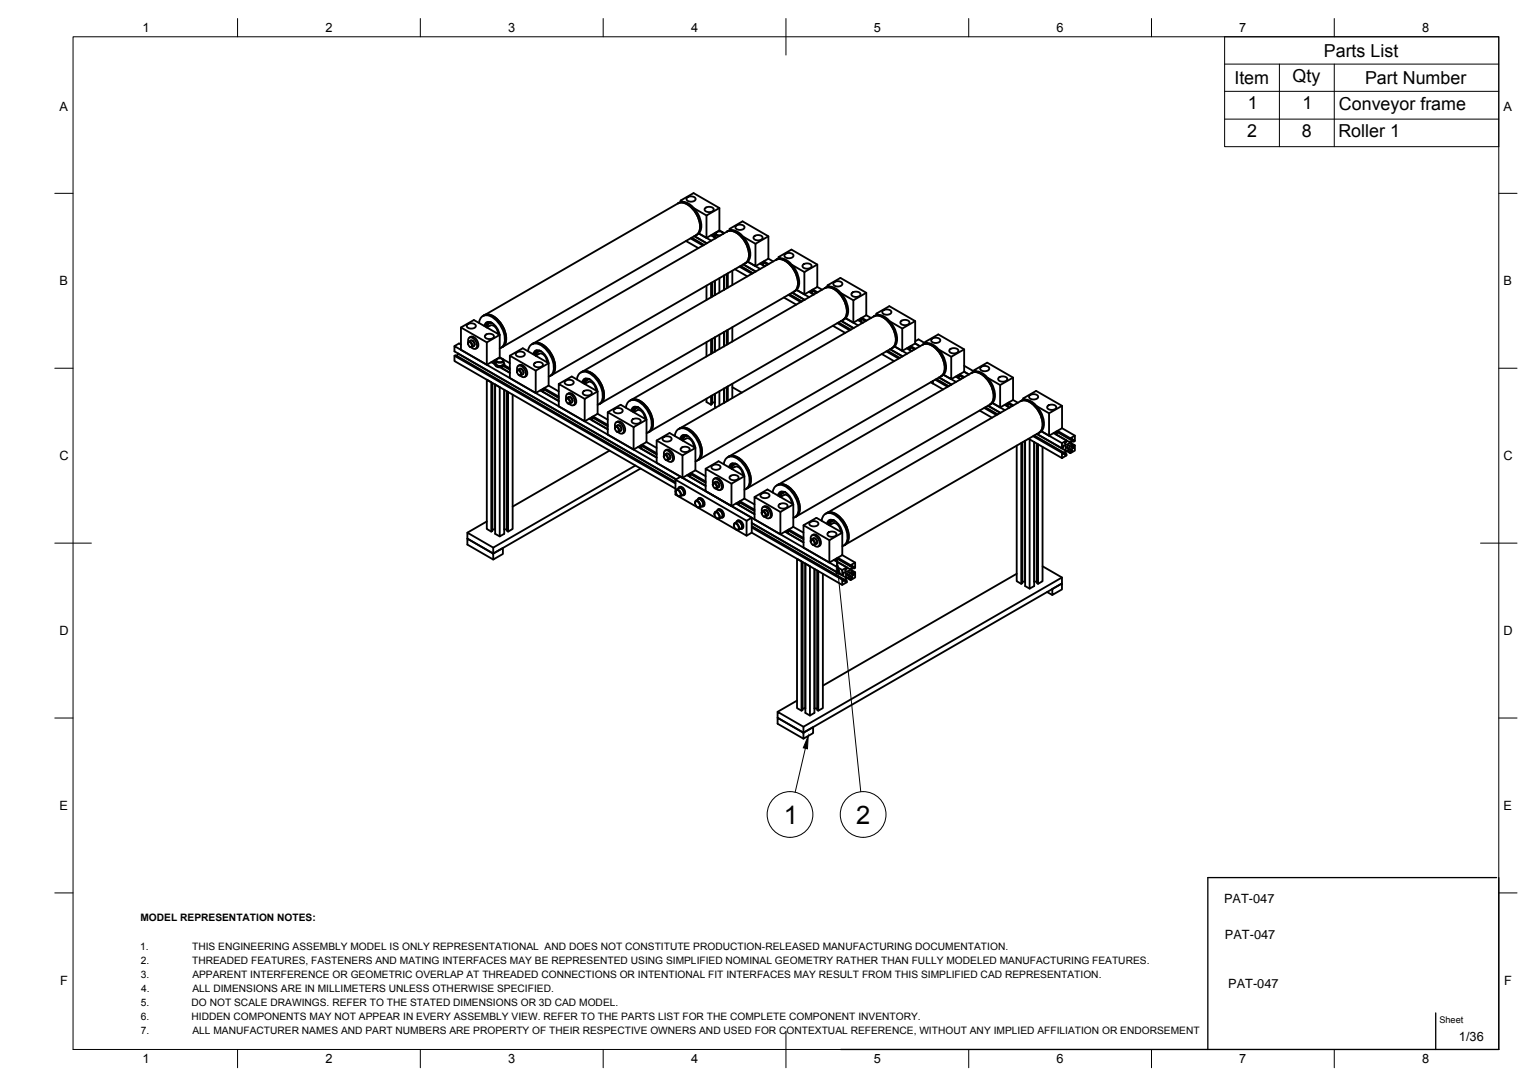
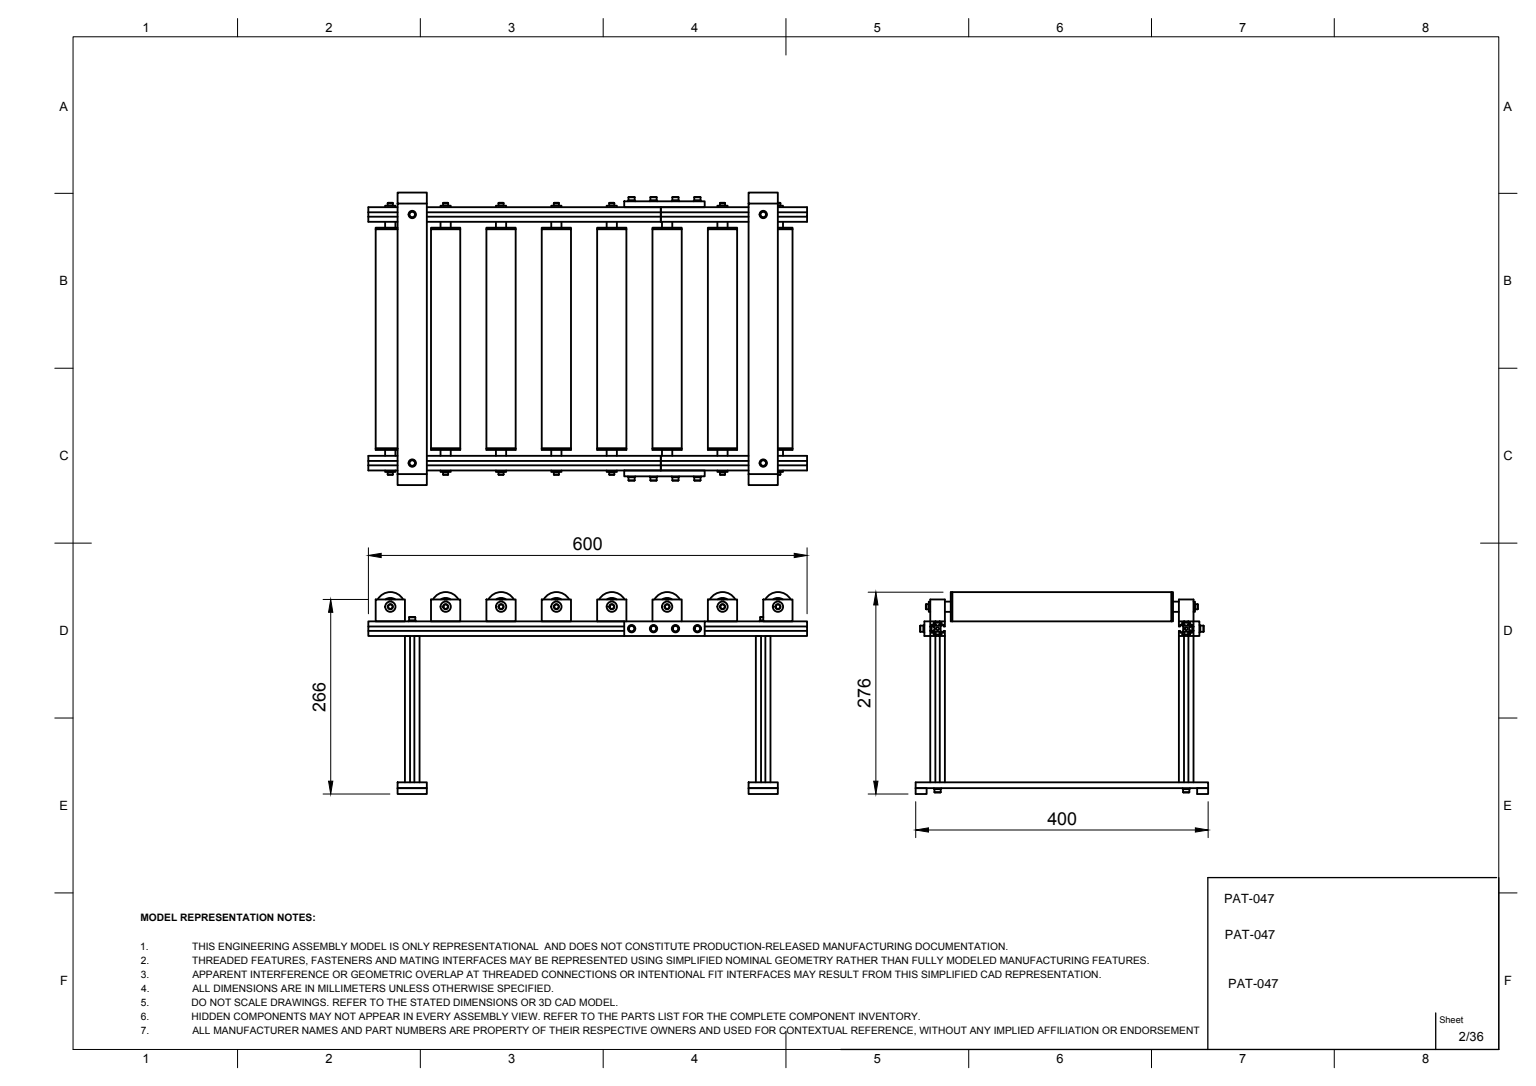
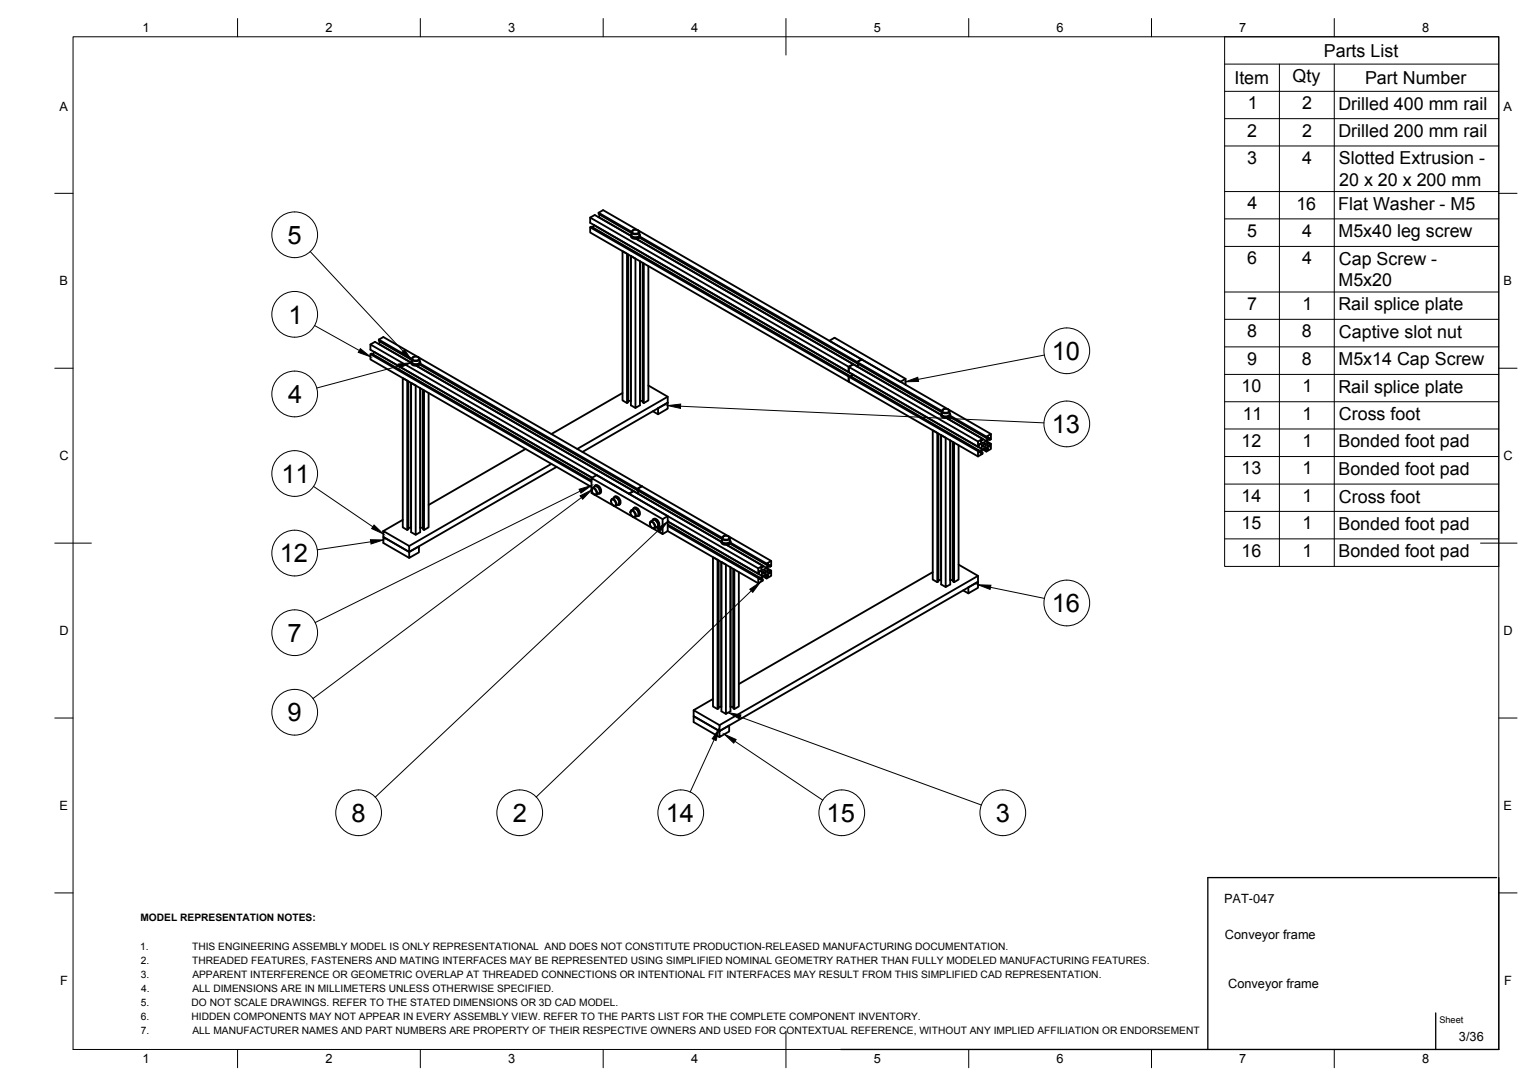
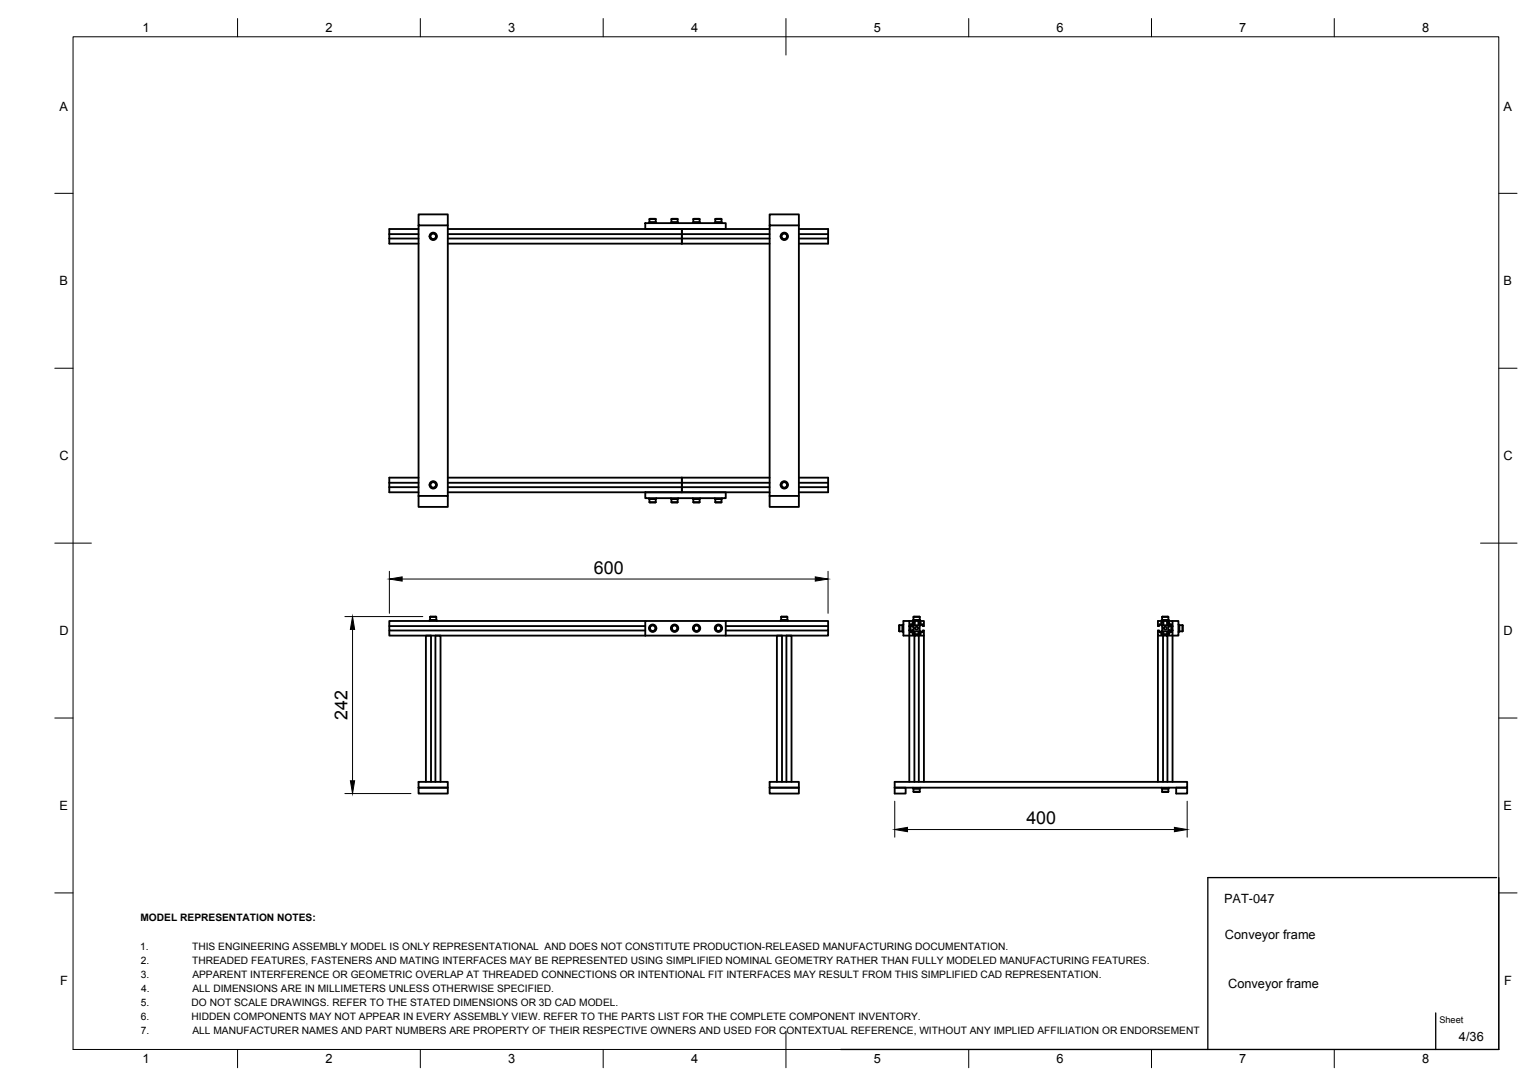
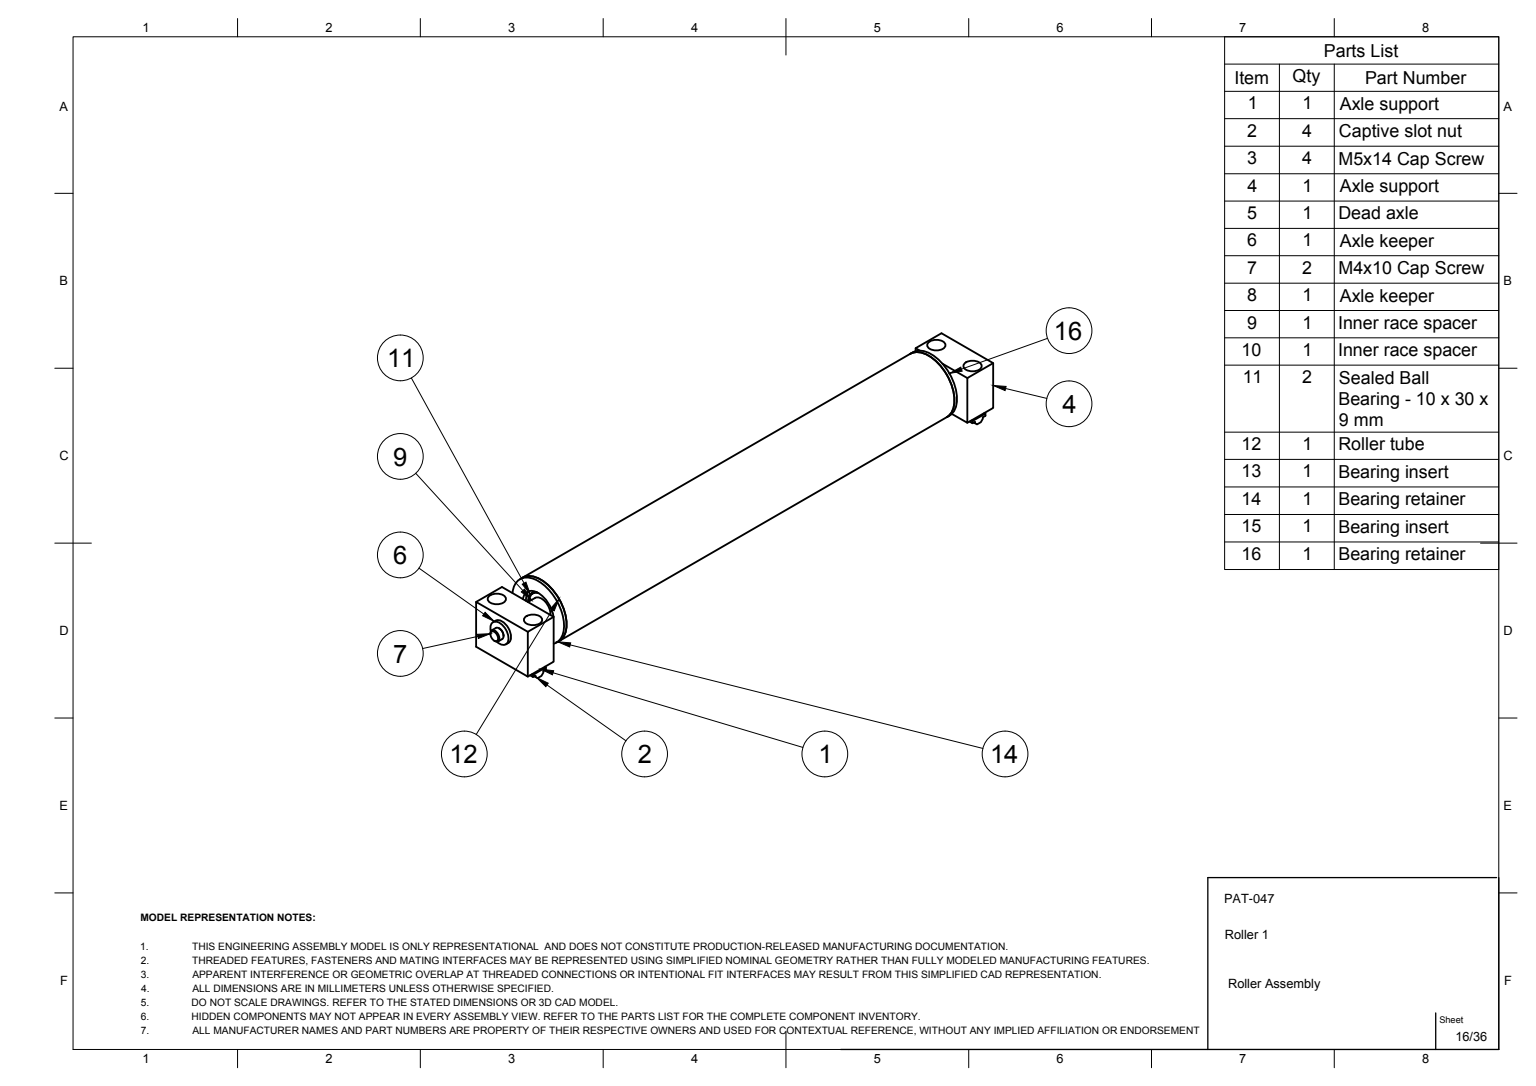
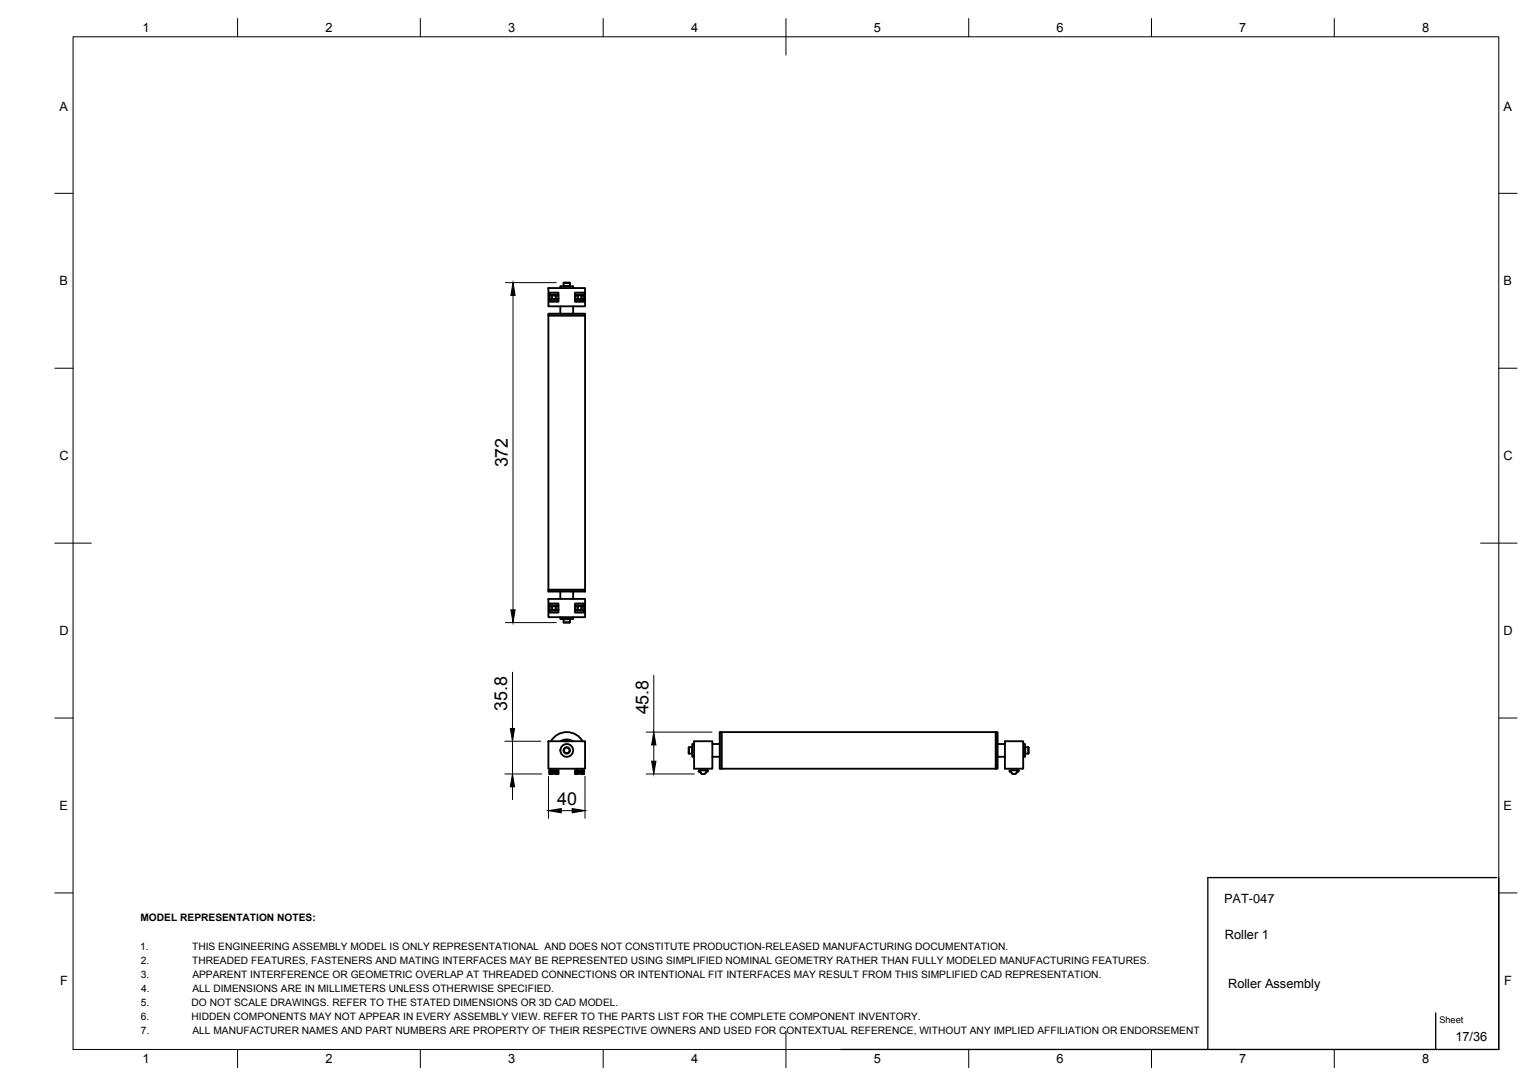
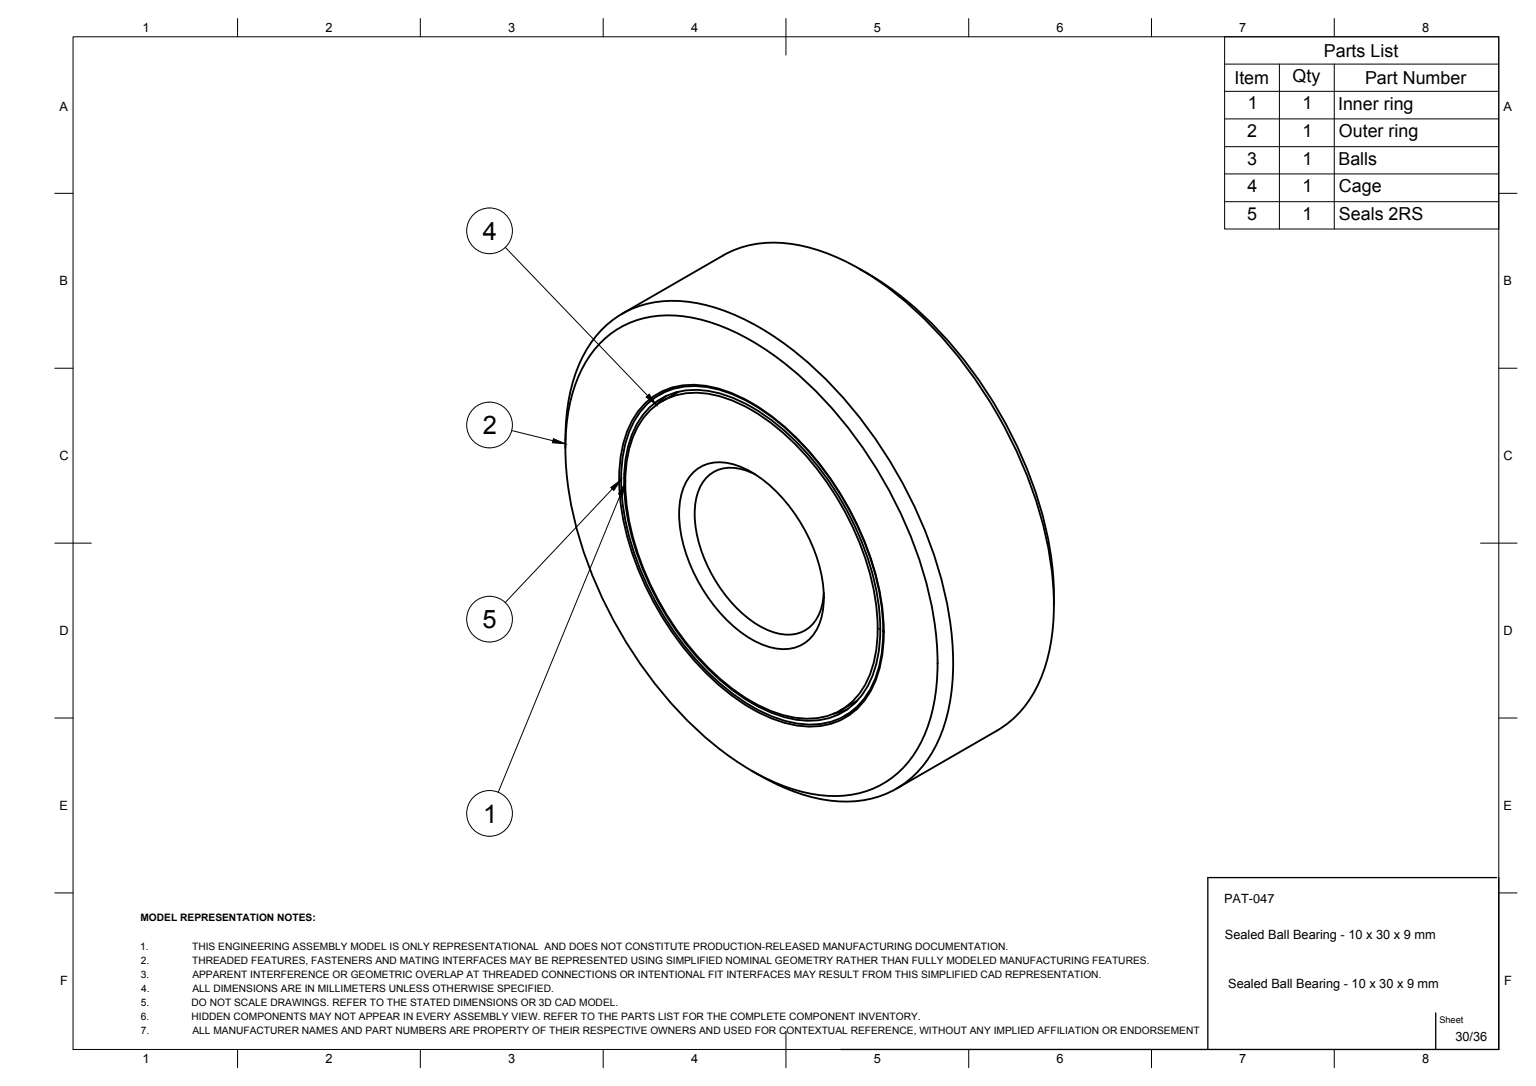
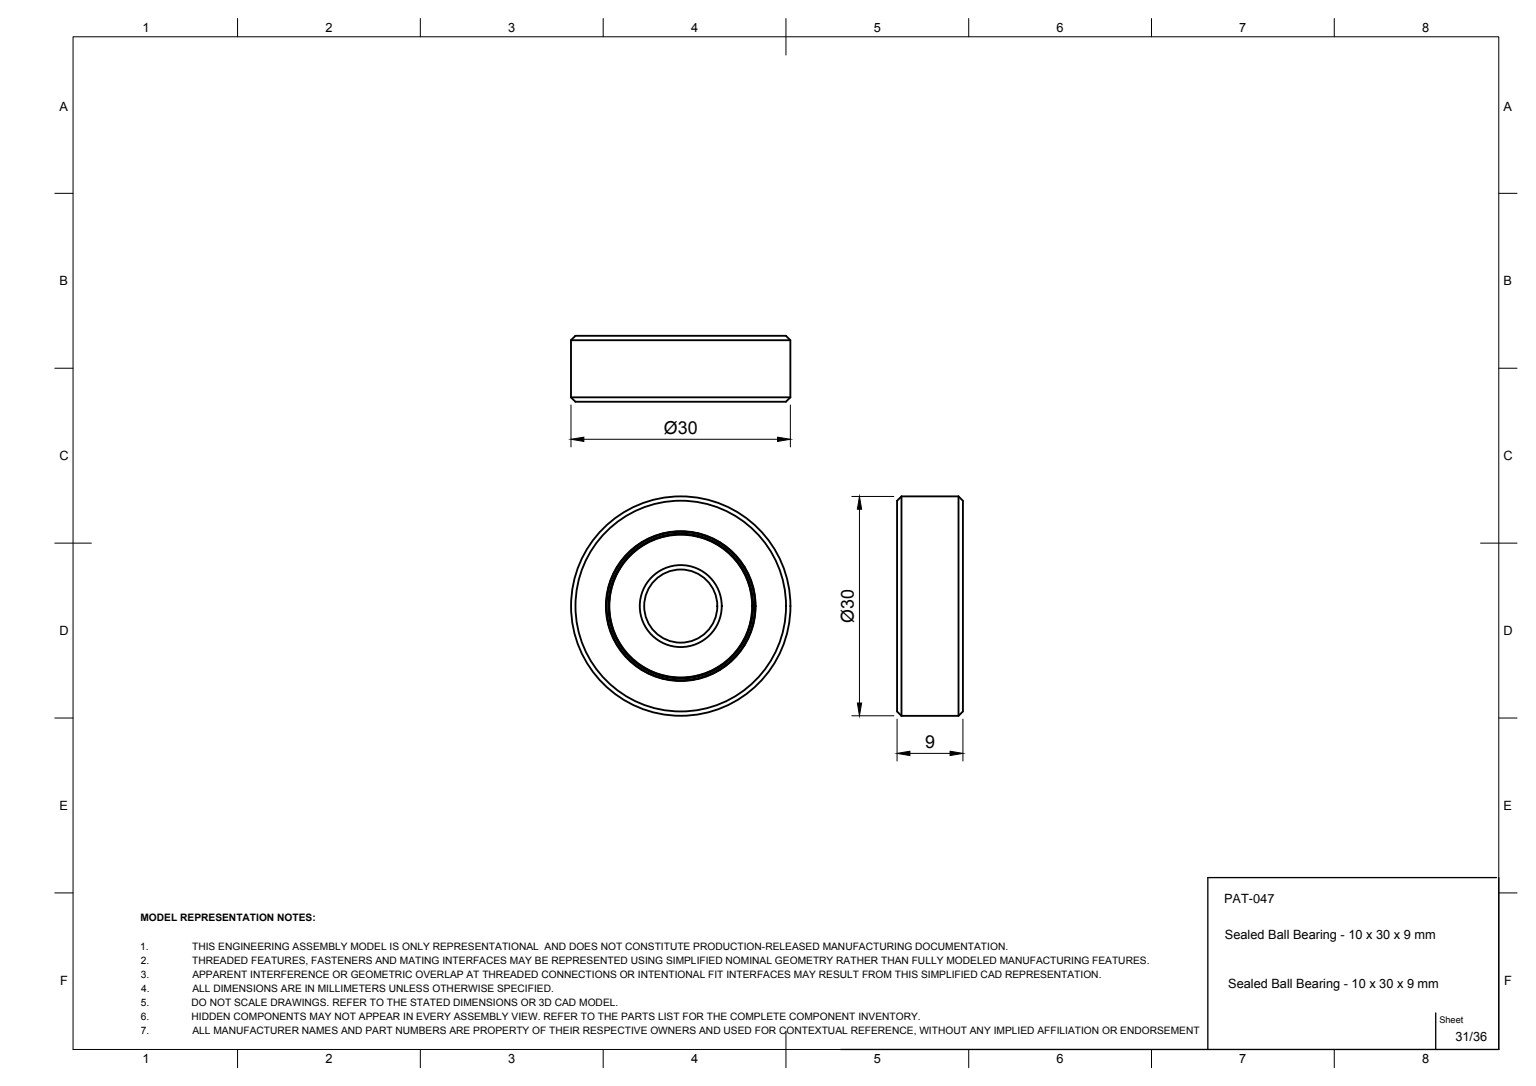
ISO-10303-21;
HEADER;
/* Generated by software containing ST-Developer
 * from STEP Tools, Inc. (www.steptools.com) 
 */

FILE_DESCRIPTION(
/* description */ ('Gravity roller conveyor section'),
/* implementation_level */ '2;1');

FILE_NAME(
/* name */ 'PAT-047',
/* time_stamp */ '2026-11-02T07:43:02-08:00',
/* author */ (''),
/* organization */ (''),
/* preprocessor_version */ 'ST-DEVELOPER v20.2',
/* originating_system */ 'Autodesk Translation Framework v15.17.0.0',
/* authorisation */ '');

FILE_SCHEMA (('AUTOMOTIVE_DESIGN { 1 0 10303 214 3 1 1 }'));
ENDSEC;

DATA;
#10=MECHANICAL_DESIGN_GEOMETRIC_PRESENTATION_REPRESENTATION('',(#529,#530,
#531,#532,#533,#534,#535,#536,#537,#538,#539,#540,#541,#542,#543,#544,#545,
#546,#547,#548,#549,#550,#551,#552,#553,#554,#555,#556,#557,#558,#559,#560,
#561,#562,#563,#564,#565,#566,#567,#568,#569,#570),#13821);
#11=ELLIPSE('',#8670,0.299389011154384,0.2117);
#12=ELLIPSE('',#8674,0.299389011154384,0.2117);
#13=ITEM_DEFINED_TRANSFORMATION($,$,#8484,#8612);
#14=ITEM_DEFINED_TRANSFORMATION($,$,#8504,#8613);
#15=ITEM_DEFINED_TRANSFORMATION($,$,#8524,#8614);
#16=ITEM_DEFINED_TRANSFORMATION($,$,#8541,#8615);
#17=ITEM_DEFINED_TRANSFORMATION($,$,#8595,#8616);
#18=ITEM_DEFINED_TRANSFORMATION($,$,#8069,#8704);
#19=ITEM_DEFINED_TRANSFORMATION($,$,#8123,#8705);
#20=ITEM_DEFINED_TRANSFORMATION($,$,#8177,#8706);
#21=ITEM_DEFINED_TRANSFORMATION($,$,#8300,#8707);
#22=ITEM_DEFINED_TRANSFORMATION($,$,#8227,#8708);
#23=ITEM_DEFINED_TRANSFORMATION($,$,#8300,#8709);
#24=ITEM_DEFINED_TRANSFORMATION($,$,#8255,#8710);
#25=ITEM_DEFINED_TRANSFORMATION($,$,#8177,#8711);
#26=ITEM_DEFINED_TRANSFORMATION($,$,#8300,#8712);
#27=ITEM_DEFINED_TRANSFORMATION($,$,#8227,#8713);
#28=ITEM_DEFINED_TRANSFORMATION($,$,#8300,#8714);
#29=ITEM_DEFINED_TRANSFORMATION($,$,#8255,#8715);
#30=ITEM_DEFINED_TRANSFORMATION($,$,#8050,#8716);
#31=ITEM_DEFINED_TRANSFORMATION($,$,#8659,#8717);
#32=ITEM_DEFINED_TRANSFORMATION($,$,#8300,#8718);
#33=ITEM_DEFINED_TRANSFORMATION($,$,#8680,#8719);
#34=ITEM_DEFINED_TRANSFORMATION($,$,#8659,#8720);
#35=ITEM_DEFINED_TRANSFORMATION($,$,#8300,#8721);
#36=ITEM_DEFINED_TRANSFORMATION($,$,#8680,#8722);
#37=ITEM_DEFINED_TRANSFORMATION($,$,#8659,#8723);
#38=ITEM_DEFINED_TRANSFORMATION($,$,#8300,#8724);
#39=ITEM_DEFINED_TRANSFORMATION($,$,#8680,#8725);
#40=ITEM_DEFINED_TRANSFORMATION($,$,#8659,#8726);
#41=ITEM_DEFINED_TRANSFORMATION($,$,#8300,#8727);
#42=ITEM_DEFINED_TRANSFORMATION($,$,#8680,#8728);
#43=ITEM_DEFINED_TRANSFORMATION($,$,#8069,#8729);
#44=ITEM_DEFINED_TRANSFORMATION($,$,#8123,#8730);
#45=ITEM_DEFINED_TRANSFORMATION($,$,#8177,#8731);
#46=ITEM_DEFINED_TRANSFORMATION($,$,#8300,#8732);
#47=ITEM_DEFINED_TRANSFORMATION($,$,#8227,#8733);
#48=ITEM_DEFINED_TRANSFORMATION($,$,#8300,#8734);
#49=ITEM_DEFINED_TRANSFORMATION($,$,#8255,#8735);
#50=ITEM_DEFINED_TRANSFORMATION($,$,#8177,#8736);
#51=ITEM_DEFINED_TRANSFORMATION($,$,#8300,#8737);
#52=ITEM_DEFINED_TRANSFORMATION($,$,#8227,#8738);
#53=ITEM_DEFINED_TRANSFORMATION($,$,#8300,#8739);
#54=ITEM_DEFINED_TRANSFORMATION($,$,#8255,#8740);
#55=ITEM_DEFINED_TRANSFORMATION($,$,#8281,#8741);
#56=ITEM_DEFINED_TRANSFORMATION($,$,#8659,#8742);
#57=ITEM_DEFINED_TRANSFORMATION($,$,#8300,#8743);
#58=ITEM_DEFINED_TRANSFORMATION($,$,#8680,#8744);
#59=ITEM_DEFINED_TRANSFORMATION($,$,#8659,#8745);
#60=ITEM_DEFINED_TRANSFORMATION($,$,#8300,#8746);
#61=ITEM_DEFINED_TRANSFORMATION($,$,#8680,#8747);
#62=ITEM_DEFINED_TRANSFORMATION($,$,#8659,#8748);
#63=ITEM_DEFINED_TRANSFORMATION($,$,#8300,#8749);
#64=ITEM_DEFINED_TRANSFORMATION($,$,#8680,#8750);
#65=ITEM_DEFINED_TRANSFORMATION($,$,#8659,#8751);
#66=ITEM_DEFINED_TRANSFORMATION($,$,#8300,#8752);
#67=ITEM_DEFINED_TRANSFORMATION($,$,#8680,#8753);
#68=ITEM_DEFINED_TRANSFORMATION($,$,#8311,#8754);
#69=ITEM_DEFINED_TRANSFORMATION($,$,#8324,#8755);
#70=ITEM_DEFINED_TRANSFORMATION($,$,#8331,#8756);
#71=ITEM_DEFINED_TRANSFORMATION($,$,#8338,#8757);
#72=ITEM_DEFINED_TRANSFORMATION($,$,#8351,#8758);
#73=ITEM_DEFINED_TRANSFORMATION($,$,#8358,#8759);
#74=ITEM_DEFINED_TRANSFORMATION($,$,#8366,#8784);
#75=ITEM_DEFINED_TRANSFORMATION($,$,#8375,#8785);
#76=ITEM_DEFINED_TRANSFORMATION($,$,#8388,#8786);
#77=ITEM_DEFINED_TRANSFORMATION($,$,#8401,#8787);
#78=ITEM_DEFINED_TRANSFORMATION($,$,#8414,#8788);
#79=ITEM_DEFINED_TRANSFORMATION($,$,#8427,#8789);
#80=ITEM_DEFINED_TRANSFORMATION($,$,#8441,#8790);
#81=ITEM_DEFINED_TRANSFORMATION($,$,#8465,#8791);
#82=ITEM_DEFINED_TRANSFORMATION($,$,#8474,#8792);
#83=ITEM_DEFINED_TRANSFORMATION($,$,#8483,#8793);
#84=ITEM_DEFINED_TRANSFORMATION($,$,#8626,#8794);
#85=ITEM_DEFINED_TRANSFORMATION($,$,#8659,#8795);
#86=ITEM_DEFINED_TRANSFORMATION($,$,#8680,#8796);
#87=ITEM_DEFINED_TRANSFORMATION($,$,#8680,#8797);
#88=ITEM_DEFINED_TRANSFORMATION($,$,#8659,#8798);
#89=ITEM_DEFINED_TRANSFORMATION($,$,#8483,#8799);
#90=ITEM_DEFINED_TRANSFORMATION($,$,#8617,#8800);
#91=ITEM_DEFINED_TRANSFORMATION($,$,#8626,#8801);
#92=ITEM_DEFINED_TRANSFORMATION($,$,#8650,#8802);
#93=ITEM_DEFINED_TRANSFORMATION($,$,#8659,#8803);
#94=ITEM_DEFINED_TRANSFORMATION($,$,#8680,#8804);
#95=ITEM_DEFINED_TRANSFORMATION($,$,#8659,#8805);
#96=ITEM_DEFINED_TRANSFORMATION($,$,#8680,#8806);
#97=ITEM_DEFINED_TRANSFORMATION($,$,#8760,#8807);
#98=ITEM_DEFINED_TRANSFORMATION($,$,#8049,#8808);
#99=ITEM_DEFINED_TRANSFORMATION($,$,#8365,#8809);
#100=ITEM_DEFINED_TRANSFORMATION($,$,#8365,#8810);
#101=ITEM_DEFINED_TRANSFORMATION($,$,#8365,#8811);
#102=ITEM_DEFINED_TRANSFORMATION($,$,#8365,#8812);
#103=ITEM_DEFINED_TRANSFORMATION($,$,#8365,#8813);
#104=ITEM_DEFINED_TRANSFORMATION($,$,#8365,#8814);
#105=ITEM_DEFINED_TRANSFORMATION($,$,#8365,#8815);
#106=ITEM_DEFINED_TRANSFORMATION($,$,#8365,#8816);
#107=(
REPRESENTATION_RELATIONSHIP($,$,#14023,#14022)
REPRESENTATION_RELATIONSHIP_WITH_TRANSFORMATION(#13)
SHAPE_REPRESENTATION_RELATIONSHIP()
);
#108=(
REPRESENTATION_RELATIONSHIP($,$,#14024,#14022)
REPRESENTATION_RELATIONSHIP_WITH_TRANSFORMATION(#14)
SHAPE_REPRESENTATION_RELATIONSHIP()
);
#109=(
REPRESENTATION_RELATIONSHIP($,$,#14025,#14022)
REPRESENTATION_RELATIONSHIP_WITH_TRANSFORMATION(#15)
SHAPE_REPRESENTATION_RELATIONSHIP()
);
#110=(
REPRESENTATION_RELATIONSHIP($,$,#14026,#14022)
REPRESENTATION_RELATIONSHIP_WITH_TRANSFORMATION(#16)
SHAPE_REPRESENTATION_RELATIONSHIP()
);
#111=(
REPRESENTATION_RELATIONSHIP($,$,#14027,#14022)
REPRESENTATION_RELATIONSHIP_WITH_TRANSFORMATION(#17)
SHAPE_REPRESENTATION_RELATIONSHIP()
);
#112=(
REPRESENTATION_RELATIONSHIP($,$,#13999,#13997)
REPRESENTATION_RELATIONSHIP_WITH_TRANSFORMATION(#18)
SHAPE_REPRESENTATION_RELATIONSHIP()
);
#113=(
REPRESENTATION_RELATIONSHIP($,$,#14000,#13997)
REPRESENTATION_RELATIONSHIP_WITH_TRANSFORMATION(#19)
SHAPE_REPRESENTATION_RELATIONSHIP()
);
#114=(
REPRESENTATION_RELATIONSHIP($,$,#14001,#13997)
REPRESENTATION_RELATIONSHIP_WITH_TRANSFORMATION(#20)
SHAPE_REPRESENTATION_RELATIONSHIP()
);
#115=(
REPRESENTATION_RELATIONSHIP($,$,#14005,#13997)
REPRESENTATION_RELATIONSHIP_WITH_TRANSFORMATION(#21)
SHAPE_REPRESENTATION_RELATIONSHIP()
);
#116=(
REPRESENTATION_RELATIONSHIP($,$,#14002,#13997)
REPRESENTATION_RELATIONSHIP_WITH_TRANSFORMATION(#22)
SHAPE_REPRESENTATION_RELATIONSHIP()
);
#117=(
REPRESENTATION_RELATIONSHIP($,$,#14005,#13997)
REPRESENTATION_RELATIONSHIP_WITH_TRANSFORMATION(#23)
SHAPE_REPRESENTATION_RELATIONSHIP()
);
#118=(
REPRESENTATION_RELATIONSHIP($,$,#14003,#13997)
REPRESENTATION_RELATIONSHIP_WITH_TRANSFORMATION(#24)
SHAPE_REPRESENTATION_RELATIONSHIP()
);
#119=(
REPRESENTATION_RELATIONSHIP($,$,#14001,#13997)
REPRESENTATION_RELATIONSHIP_WITH_TRANSFORMATION(#25)
SHAPE_REPRESENTATION_RELATIONSHIP()
);
#120=(
REPRESENTATION_RELATIONSHIP($,$,#14005,#13997)
REPRESENTATION_RELATIONSHIP_WITH_TRANSFORMATION(#26)
SHAPE_REPRESENTATION_RELATIONSHIP()
);
#121=(
REPRESENTATION_RELATIONSHIP($,$,#14002,#13997)
REPRESENTATION_RELATIONSHIP_WITH_TRANSFORMATION(#27)
SHAPE_REPRESENTATION_RELATIONSHIP()
);
#122=(
REPRESENTATION_RELATIONSHIP($,$,#14005,#13997)
REPRESENTATION_RELATIONSHIP_WITH_TRANSFORMATION(#28)
SHAPE_REPRESENTATION_RELATIONSHIP()
);
#123=(
REPRESENTATION_RELATIONSHIP($,$,#14003,#13997)
REPRESENTATION_RELATIONSHIP_WITH_TRANSFORMATION(#29)
SHAPE_REPRESENTATION_RELATIONSHIP()
);
#124=(
REPRESENTATION_RELATIONSHIP($,$,#13998,#13997)
REPRESENTATION_RELATIONSHIP_WITH_TRANSFORMATION(#30)
SHAPE_REPRESENTATION_RELATIONSHIP()
);
#125=(
REPRESENTATION_RELATIONSHIP($,$,#14031,#13997)
REPRESENTATION_RELATIONSHIP_WITH_TRANSFORMATION(#31)
SHAPE_REPRESENTATION_RELATIONSHIP()
);
#126=(
REPRESENTATION_RELATIONSHIP($,$,#14005,#13997)
REPRESENTATION_RELATIONSHIP_WITH_TRANSFORMATION(#32)
SHAPE_REPRESENTATION_RELATIONSHIP()
);
#127=(
REPRESENTATION_RELATIONSHIP($,$,#14032,#13997)
REPRESENTATION_RELATIONSHIP_WITH_TRANSFORMATION(#33)
SHAPE_REPRESENTATION_RELATIONSHIP()
);
#128=(
REPRESENTATION_RELATIONSHIP($,$,#14031,#13997)
REPRESENTATION_RELATIONSHIP_WITH_TRANSFORMATION(#34)
SHAPE_REPRESENTATION_RELATIONSHIP()
);
#129=(
REPRESENTATION_RELATIONSHIP($,$,#14005,#13997)
REPRESENTATION_RELATIONSHIP_WITH_TRANSFORMATION(#35)
SHAPE_REPRESENTATION_RELATIONSHIP()
);
#130=(
REPRESENTATION_RELATIONSHIP($,$,#14032,#13997)
REPRESENTATION_RELATIONSHIP_WITH_TRANSFORMATION(#36)
SHAPE_REPRESENTATION_RELATIONSHIP()
);
#131=(
REPRESENTATION_RELATIONSHIP($,$,#14031,#13997)
REPRESENTATION_RELATIONSHIP_WITH_TRANSFORMATION(#37)
SHAPE_REPRESENTATION_RELATIONSHIP()
);
#132=(
REPRESENTATION_RELATIONSHIP($,$,#14005,#13997)
REPRESENTATION_RELATIONSHIP_WITH_TRANSFORMATION(#38)
SHAPE_REPRESENTATION_RELATIONSHIP()
);
#133=(
REPRESENTATION_RELATIONSHIP($,$,#14032,#13997)
REPRESENTATION_RELATIONSHIP_WITH_TRANSFORMATION(#39)
SHAPE_REPRESENTATION_RELATIONSHIP()
);
#134=(
REPRESENTATION_RELATIONSHIP($,$,#14031,#13997)
REPRESENTATION_RELATIONSHIP_WITH_TRANSFORMATION(#40)
SHAPE_REPRESENTATION_RELATIONSHIP()
);
#135=(
REPRESENTATION_RELATIONSHIP($,$,#14005,#13997)
REPRESENTATION_RELATIONSHIP_WITH_TRANSFORMATION(#41)
SHAPE_REPRESENTATION_RELATIONSHIP()
);
#136=(
REPRESENTATION_RELATIONSHIP($,$,#14032,#13997)
REPRESENTATION_RELATIONSHIP_WITH_TRANSFORMATION(#42)
SHAPE_REPRESENTATION_RELATIONSHIP()
);
#137=(
REPRESENTATION_RELATIONSHIP($,$,#13999,#13997)
REPRESENTATION_RELATIONSHIP_WITH_TRANSFORMATION(#43)
SHAPE_REPRESENTATION_RELATIONSHIP()
);
#138=(
REPRESENTATION_RELATIONSHIP($,$,#14000,#13997)
REPRESENTATION_RELATIONSHIP_WITH_TRANSFORMATION(#44)
SHAPE_REPRESENTATION_RELATIONSHIP()
);
#139=(
REPRESENTATION_RELATIONSHIP($,$,#14001,#13997)
REPRESENTATION_RELATIONSHIP_WITH_TRANSFORMATION(#45)
SHAPE_REPRESENTATION_RELATIONSHIP()
);
#140=(
REPRESENTATION_RELATIONSHIP($,$,#14005,#13997)
REPRESENTATION_RELATIONSHIP_WITH_TRANSFORMATION(#46)
SHAPE_REPRESENTATION_RELATIONSHIP()
);
#141=(
REPRESENTATION_RELATIONSHIP($,$,#14002,#13997)
REPRESENTATION_RELATIONSHIP_WITH_TRANSFORMATION(#47)
SHAPE_REPRESENTATION_RELATIONSHIP()
);
#142=(
REPRESENTATION_RELATIONSHIP($,$,#14005,#13997)
REPRESENTATION_RELATIONSHIP_WITH_TRANSFORMATION(#48)
SHAPE_REPRESENTATION_RELATIONSHIP()
);
#143=(
REPRESENTATION_RELATIONSHIP($,$,#14003,#13997)
REPRESENTATION_RELATIONSHIP_WITH_TRANSFORMATION(#49)
SHAPE_REPRESENTATION_RELATIONSHIP()
);
#144=(
REPRESENTATION_RELATIONSHIP($,$,#14001,#13997)
REPRESENTATION_RELATIONSHIP_WITH_TRANSFORMATION(#50)
SHAPE_REPRESENTATION_RELATIONSHIP()
);
#145=(
REPRESENTATION_RELATIONSHIP($,$,#14005,#13997)
REPRESENTATION_RELATIONSHIP_WITH_TRANSFORMATION(#51)
SHAPE_REPRESENTATION_RELATIONSHIP()
);
#146=(
REPRESENTATION_RELATIONSHIP($,$,#14002,#13997)
REPRESENTATION_RELATIONSHIP_WITH_TRANSFORMATION(#52)
SHAPE_REPRESENTATION_RELATIONSHIP()
);
#147=(
REPRESENTATION_RELATIONSHIP($,$,#14005,#13997)
REPRESENTATION_RELATIONSHIP_WITH_TRANSFORMATION(#53)
SHAPE_REPRESENTATION_RELATIONSHIP()
);
#148=(
REPRESENTATION_RELATIONSHIP($,$,#14003,#13997)
REPRESENTATION_RELATIONSHIP_WITH_TRANSFORMATION(#54)
SHAPE_REPRESENTATION_RELATIONSHIP()
);
#149=(
REPRESENTATION_RELATIONSHIP($,$,#14004,#13997)
REPRESENTATION_RELATIONSHIP_WITH_TRANSFORMATION(#55)
SHAPE_REPRESENTATION_RELATIONSHIP()
);
#150=(
REPRESENTATION_RELATIONSHIP($,$,#14031,#13997)
REPRESENTATION_RELATIONSHIP_WITH_TRANSFORMATION(#56)
SHAPE_REPRESENTATION_RELATIONSHIP()
);
#151=(
REPRESENTATION_RELATIONSHIP($,$,#14005,#13997)
REPRESENTATION_RELATIONSHIP_WITH_TRANSFORMATION(#57)
SHAPE_REPRESENTATION_RELATIONSHIP()
);
#152=(
REPRESENTATION_RELATIONSHIP($,$,#14032,#13997)
REPRESENTATION_RELATIONSHIP_WITH_TRANSFORMATION(#58)
SHAPE_REPRESENTATION_RELATIONSHIP()
);
#153=(
REPRESENTATION_RELATIONSHIP($,$,#14031,#13997)
REPRESENTATION_RELATIONSHIP_WITH_TRANSFORMATION(#59)
SHAPE_REPRESENTATION_RELATIONSHIP()
);
#154=(
REPRESENTATION_RELATIONSHIP($,$,#14005,#13997)
REPRESENTATION_RELATIONSHIP_WITH_TRANSFORMATION(#60)
SHAPE_REPRESENTATION_RELATIONSHIP()
);
#155=(
REPRESENTATION_RELATIONSHIP($,$,#14032,#13997)
REPRESENTATION_RELATIONSHIP_WITH_TRANSFORMATION(#61)
SHAPE_REPRESENTATION_RELATIONSHIP()
);
#156=(
REPRESENTATION_RELATIONSHIP($,$,#14031,#13997)
REPRESENTATION_RELATIONSHIP_WITH_TRANSFORMATION(#62)
SHAPE_REPRESENTATION_RELATIONSHIP()
);
#157=(
REPRESENTATION_RELATIONSHIP($,$,#14005,#13997)
REPRESENTATION_RELATIONSHIP_WITH_TRANSFORMATION(#63)
SHAPE_REPRESENTATION_RELATIONSHIP()
);
#158=(
REPRESENTATION_RELATIONSHIP($,$,#14032,#13997)
REPRESENTATION_RELATIONSHIP_WITH_TRANSFORMATION(#64)
SHAPE_REPRESENTATION_RELATIONSHIP()
);
#159=(
REPRESENTATION_RELATIONSHIP($,$,#14031,#13997)
REPRESENTATION_RELATIONSHIP_WITH_TRANSFORMATION(#65)
SHAPE_REPRESENTATION_RELATIONSHIP()
);
#160=(
REPRESENTATION_RELATIONSHIP($,$,#14005,#13997)
REPRESENTATION_RELATIONSHIP_WITH_TRANSFORMATION(#66)
SHAPE_REPRESENTATION_RELATIONSHIP()
);
#161=(
REPRESENTATION_RELATIONSHIP($,$,#14032,#13997)
REPRESENTATION_RELATIONSHIP_WITH_TRANSFORMATION(#67)
SHAPE_REPRESENTATION_RELATIONSHIP()
);
#162=(
REPRESENTATION_RELATIONSHIP($,$,#14006,#13997)
REPRESENTATION_RELATIONSHIP_WITH_TRANSFORMATION(#68)
SHAPE_REPRESENTATION_RELATIONSHIP()
);
#163=(
REPRESENTATION_RELATIONSHIP($,$,#14007,#13997)
REPRESENTATION_RELATIONSHIP_WITH_TRANSFORMATION(#69)
SHAPE_REPRESENTATION_RELATIONSHIP()
);
#164=(
REPRESENTATION_RELATIONSHIP($,$,#14008,#13997)
REPRESENTATION_RELATIONSHIP_WITH_TRANSFORMATION(#70)
SHAPE_REPRESENTATION_RELATIONSHIP()
);
#165=(
REPRESENTATION_RELATIONSHIP($,$,#14009,#13997)
REPRESENTATION_RELATIONSHIP_WITH_TRANSFORMATION(#71)
SHAPE_REPRESENTATION_RELATIONSHIP()
);
#166=(
REPRESENTATION_RELATIONSHIP($,$,#14010,#13997)
REPRESENTATION_RELATIONSHIP_WITH_TRANSFORMATION(#72)
SHAPE_REPRESENTATION_RELATIONSHIP()
);
#167=(
REPRESENTATION_RELATIONSHIP($,$,#14011,#13997)
REPRESENTATION_RELATIONSHIP_WITH_TRANSFORMATION(#73)
SHAPE_REPRESENTATION_RELATIONSHIP()
);
#168=(
REPRESENTATION_RELATIONSHIP($,$,#14013,#14012)
REPRESENTATION_RELATIONSHIP_WITH_TRANSFORMATION(#74)
SHAPE_REPRESENTATION_RELATIONSHIP()
);
#169=(
REPRESENTATION_RELATIONSHIP($,$,#14014,#14012)
REPRESENTATION_RELATIONSHIP_WITH_TRANSFORMATION(#75)
SHAPE_REPRESENTATION_RELATIONSHIP()
);
#170=(
REPRESENTATION_RELATIONSHIP($,$,#14015,#14012)
REPRESENTATION_RELATIONSHIP_WITH_TRANSFORMATION(#76)
SHAPE_REPRESENTATION_RELATIONSHIP()
);
#171=(
REPRESENTATION_RELATIONSHIP($,$,#14016,#14012)
REPRESENTATION_RELATIONSHIP_WITH_TRANSFORMATION(#77)
SHAPE_REPRESENTATION_RELATIONSHIP()
);
#172=(
REPRESENTATION_RELATIONSHIP($,$,#14017,#14012)
REPRESENTATION_RELATIONSHIP_WITH_TRANSFORMATION(#78)
SHAPE_REPRESENTATION_RELATIONSHIP()
);
#173=(
REPRESENTATION_RELATIONSHIP($,$,#14018,#14012)
REPRESENTATION_RELATIONSHIP_WITH_TRANSFORMATION(#79)
SHAPE_REPRESENTATION_RELATIONSHIP()
);
#174=(
REPRESENTATION_RELATIONSHIP($,$,#14019,#14012)
REPRESENTATION_RELATIONSHIP_WITH_TRANSFORMATION(#80)
SHAPE_REPRESENTATION_RELATIONSHIP()
);
#175=(
REPRESENTATION_RELATIONSHIP($,$,#14020,#14012)
REPRESENTATION_RELATIONSHIP_WITH_TRANSFORMATION(#81)
SHAPE_REPRESENTATION_RELATIONSHIP()
);
#176=(
REPRESENTATION_RELATIONSHIP($,$,#14021,#14012)
REPRESENTATION_RELATIONSHIP_WITH_TRANSFORMATION(#82)
SHAPE_REPRESENTATION_RELATIONSHIP()
);
#177=(
REPRESENTATION_RELATIONSHIP($,$,#14022,#14012)
REPRESENTATION_RELATIONSHIP_WITH_TRANSFORMATION(#83)
SHAPE_REPRESENTATION_RELATIONSHIP()
);
#178=(
REPRESENTATION_RELATIONSHIP($,$,#14029,#14012)
REPRESENTATION_RELATIONSHIP_WITH_TRANSFORMATION(#84)
SHAPE_REPRESENTATION_RELATIONSHIP()
);
#179=(
REPRESENTATION_RELATIONSHIP($,$,#14031,#14012)
REPRESENTATION_RELATIONSHIP_WITH_TRANSFORMATION(#85)
SHAPE_REPRESENTATION_RELATIONSHIP()
);
#180=(
REPRESENTATION_RELATIONSHIP($,$,#14032,#14012)
REPRESENTATION_RELATIONSHIP_WITH_TRANSFORMATION(#86)
SHAPE_REPRESENTATION_RELATIONSHIP()
);
#181=(
REPRESENTATION_RELATIONSHIP($,$,#14032,#14012)
REPRESENTATION_RELATIONSHIP_WITH_TRANSFORMATION(#87)
SHAPE_REPRESENTATION_RELATIONSHIP()
);
#182=(
REPRESENTATION_RELATIONSHIP($,$,#14031,#14012)
REPRESENTATION_RELATIONSHIP_WITH_TRANSFORMATION(#88)
SHAPE_REPRESENTATION_RELATIONSHIP()
);
#183=(
REPRESENTATION_RELATIONSHIP($,$,#14022,#14012)
REPRESENTATION_RELATIONSHIP_WITH_TRANSFORMATION(#89)
SHAPE_REPRESENTATION_RELATIONSHIP()
);
#184=(
REPRESENTATION_RELATIONSHIP($,$,#14028,#14012)
REPRESENTATION_RELATIONSHIP_WITH_TRANSFORMATION(#90)
SHAPE_REPRESENTATION_RELATIONSHIP()
);
#185=(
REPRESENTATION_RELATIONSHIP($,$,#14029,#14012)
REPRESENTATION_RELATIONSHIP_WITH_TRANSFORMATION(#91)
SHAPE_REPRESENTATION_RELATIONSHIP()
);
#186=(
REPRESENTATION_RELATIONSHIP($,$,#14030,#14012)
REPRESENTATION_RELATIONSHIP_WITH_TRANSFORMATION(#92)
SHAPE_REPRESENTATION_RELATIONSHIP()
);
#187=(
REPRESENTATION_RELATIONSHIP($,$,#14031,#14012)
REPRESENTATION_RELATIONSHIP_WITH_TRANSFORMATION(#93)
SHAPE_REPRESENTATION_RELATIONSHIP()
);
#188=(
REPRESENTATION_RELATIONSHIP($,$,#14032,#14012)
REPRESENTATION_RELATIONSHIP_WITH_TRANSFORMATION(#94)
SHAPE_REPRESENTATION_RELATIONSHIP()
);
#189=(
REPRESENTATION_RELATIONSHIP($,$,#14031,#14012)
REPRESENTATION_RELATIONSHIP_WITH_TRANSFORMATION(#95)
SHAPE_REPRESENTATION_RELATIONSHIP()
);
#190=(
REPRESENTATION_RELATIONSHIP($,$,#14032,#14012)
REPRESENTATION_RELATIONSHIP_WITH_TRANSFORMATION(#96)
SHAPE_REPRESENTATION_RELATIONSHIP()
);
#191=(
REPRESENTATION_RELATIONSHIP($,$,#14033,#14012)
REPRESENTATION_RELATIONSHIP_WITH_TRANSFORMATION(#97)
SHAPE_REPRESENTATION_RELATIONSHIP()
);
#192=(
REPRESENTATION_RELATIONSHIP($,$,#13997,#13996)
REPRESENTATION_RELATIONSHIP_WITH_TRANSFORMATION(#98)
SHAPE_REPRESENTATION_RELATIONSHIP()
);
#193=(
REPRESENTATION_RELATIONSHIP($,$,#14012,#13996)
REPRESENTATION_RELATIONSHIP_WITH_TRANSFORMATION(#99)
SHAPE_REPRESENTATION_RELATIONSHIP()
);
#194=(
REPRESENTATION_RELATIONSHIP($,$,#14012,#13996)
REPRESENTATION_RELATIONSHIP_WITH_TRANSFORMATION(#100)
SHAPE_REPRESENTATION_RELATIONSHIP()
);
#195=(
REPRESENTATION_RELATIONSHIP($,$,#14012,#13996)
REPRESENTATION_RELATIONSHIP_WITH_TRANSFORMATION(#101)
SHAPE_REPRESENTATION_RELATIONSHIP()
);
#196=(
REPRESENTATION_RELATIONSHIP($,$,#14012,#13996)
REPRESENTATION_RELATIONSHIP_WITH_TRANSFORMATION(#102)
SHAPE_REPRESENTATION_RELATIONSHIP()
);
#197=(
REPRESENTATION_RELATIONSHIP($,$,#14012,#13996)
REPRESENTATION_RELATIONSHIP_WITH_TRANSFORMATION(#103)
SHAPE_REPRESENTATION_RELATIONSHIP()
);
#198=(
REPRESENTATION_RELATIONSHIP($,$,#14012,#13996)
REPRESENTATION_RELATIONSHIP_WITH_TRANSFORMATION(#104)
SHAPE_REPRESENTATION_RELATIONSHIP()
);
#199=(
REPRESENTATION_RELATIONSHIP($,$,#14012,#13996)
REPRESENTATION_RELATIONSHIP_WITH_TRANSFORMATION(#105)
SHAPE_REPRESENTATION_RELATIONSHIP()
);
#200=(
REPRESENTATION_RELATIONSHIP($,$,#14012,#13996)
REPRESENTATION_RELATIONSHIP_WITH_TRANSFORMATION(#106)
SHAPE_REPRESENTATION_RELATIONSHIP()
);
#201=CONTEXT_DEPENDENT_SHAPE_REPRESENTATION(#107,#13896);
#202=CONTEXT_DEPENDENT_SHAPE_REPRESENTATION(#108,#13897);
#203=CONTEXT_DEPENDENT_SHAPE_REPRESENTATION(#109,#13898);
#204=CONTEXT_DEPENDENT_SHAPE_REPRESENTATION(#110,#13899);
#205=CONTEXT_DEPENDENT_SHAPE_REPRESENTATION(#111,#13900);
#206=CONTEXT_DEPENDENT_SHAPE_REPRESENTATION(#112,#13906);
#207=CONTEXT_DEPENDENT_SHAPE_REPRESENTATION(#113,#13907);
#208=CONTEXT_DEPENDENT_SHAPE_REPRESENTATION(#114,#13908);
#209=CONTEXT_DEPENDENT_SHAPE_REPRESENTATION(#115,#13909);
#210=CONTEXT_DEPENDENT_SHAPE_REPRESENTATION(#116,#13910);
#211=CONTEXT_DEPENDENT_SHAPE_REPRESENTATION(#117,#13911);
#212=CONTEXT_DEPENDENT_SHAPE_REPRESENTATION(#118,#13912);
#213=CONTEXT_DEPENDENT_SHAPE_REPRESENTATION(#119,#13913);
#214=CONTEXT_DEPENDENT_SHAPE_REPRESENTATION(#120,#13914);
#215=CONTEXT_DEPENDENT_SHAPE_REPRESENTATION(#121,#13915);
#216=CONTEXT_DEPENDENT_SHAPE_REPRESENTATION(#122,#13916);
#217=CONTEXT_DEPENDENT_SHAPE_REPRESENTATION(#123,#13917);
#218=CONTEXT_DEPENDENT_SHAPE_REPRESENTATION(#124,#13918);
#219=CONTEXT_DEPENDENT_SHAPE_REPRESENTATION(#125,#13919);
#220=CONTEXT_DEPENDENT_SHAPE_REPRESENTATION(#126,#13920);
#221=CONTEXT_DEPENDENT_SHAPE_REPRESENTATION(#127,#13921);
#222=CONTEXT_DEPENDENT_SHAPE_REPRESENTATION(#128,#13922);
#223=CONTEXT_DEPENDENT_SHAPE_REPRESENTATION(#129,#13923);
#224=CONTEXT_DEPENDENT_SHAPE_REPRESENTATION(#130,#13924);
#225=CONTEXT_DEPENDENT_SHAPE_REPRESENTATION(#131,#13925);
#226=CONTEXT_DEPENDENT_SHAPE_REPRESENTATION(#132,#13926);
#227=CONTEXT_DEPENDENT_SHAPE_REPRESENTATION(#133,#13927);
#228=CONTEXT_DEPENDENT_SHAPE_REPRESENTATION(#134,#13928);
#229=CONTEXT_DEPENDENT_SHAPE_REPRESENTATION(#135,#13929);
#230=CONTEXT_DEPENDENT_SHAPE_REPRESENTATION(#136,#13930);
#231=CONTEXT_DEPENDENT_SHAPE_REPRESENTATION(#137,#13931);
#232=CONTEXT_DEPENDENT_SHAPE_REPRESENTATION(#138,#13932);
#233=CONTEXT_DEPENDENT_SHAPE_REPRESENTATION(#139,#13933);
#234=CONTEXT_DEPENDENT_SHAPE_REPRESENTATION(#140,#13934);
#235=CONTEXT_DEPENDENT_SHAPE_REPRESENTATION(#141,#13935);
#236=CONTEXT_DEPENDENT_SHAPE_REPRESENTATION(#142,#13936);
#237=CONTEXT_DEPENDENT_SHAPE_REPRESENTATION(#143,#13937);
#238=CONTEXT_DEPENDENT_SHAPE_REPRESENTATION(#144,#13938);
#239=CONTEXT_DEPENDENT_SHAPE_REPRESENTATION(#145,#13939);
#240=CONTEXT_DEPENDENT_SHAPE_REPRESENTATION(#146,#13940);
#241=CONTEXT_DEPENDENT_SHAPE_REPRESENTATION(#147,#13941);
#242=CONTEXT_DEPENDENT_SHAPE_REPRESENTATION(#148,#13942);
#243=CONTEXT_DEPENDENT_SHAPE_REPRESENTATION(#149,#13943);
#244=CONTEXT_DEPENDENT_SHAPE_REPRESENTATION(#150,#13944);
#245=CONTEXT_DEPENDENT_SHAPE_REPRESENTATION(#151,#13945);
#246=CONTEXT_DEPENDENT_SHAPE_REPRESENTATION(#152,#13946);
#247=CONTEXT_DEPENDENT_SHAPE_REPRESENTATION(#153,#13947);
#248=CONTEXT_DEPENDENT_SHAPE_REPRESENTATION(#154,#13948);
#249=CONTEXT_DEPENDENT_SHAPE_REPRESENTATION(#155,#13949);
#250=CONTEXT_DEPENDENT_SHAPE_REPRESENTATION(#156,#13950);
#251=CONTEXT_DEPENDENT_SHAPE_REPRESENTATION(#157,#13951);
#252=CONTEXT_DEPENDENT_SHAPE_REPRESENTATION(#158,#13952);
#253=CONTEXT_DEPENDENT_SHAPE_REPRESENTATION(#159,#13953);
#254=CONTEXT_DEPENDENT_SHAPE_REPRESENTATION(#160,#13954);
#255=CONTEXT_DEPENDENT_SHAPE_REPRESENTATION(#161,#13955);
#256=CONTEXT_DEPENDENT_SHAPE_REPRESENTATION(#162,#13956);
#257=CONTEXT_DEPENDENT_SHAPE_REPRESENTATION(#163,#13957);
#258=CONTEXT_DEPENDENT_SHAPE_REPRESENTATION(#164,#13958);
#259=CONTEXT_DEPENDENT_SHAPE_REPRESENTATION(#165,#13959);
#260=CONTEXT_DEPENDENT_SHAPE_REPRESENTATION(#166,#13960);
#261=CONTEXT_DEPENDENT_SHAPE_REPRESENTATION(#167,#13961);
#262=CONTEXT_DEPENDENT_SHAPE_REPRESENTATION(#168,#13963);
#263=CONTEXT_DEPENDENT_SHAPE_REPRESENTATION(#169,#13964);
#264=CONTEXT_DEPENDENT_SHAPE_REPRESENTATION(#170,#13965);
#265=CONTEXT_DEPENDENT_SHAPE_REPRESENTATION(#171,#13966);
#266=CONTEXT_DEPENDENT_SHAPE_REPRESENTATION(#172,#13967);
#267=CONTEXT_DEPENDENT_SHAPE_REPRESENTATION(#173,#13968);
#268=CONTEXT_DEPENDENT_SHAPE_REPRESENTATION(#174,#13969);
#269=CONTEXT_DEPENDENT_SHAPE_REPRESENTATION(#175,#13970);
#270=CONTEXT_DEPENDENT_SHAPE_REPRESENTATION(#176,#13971);
#271=CONTEXT_DEPENDENT_SHAPE_REPRESENTATION(#177,#13972);
#272=CONTEXT_DEPENDENT_SHAPE_REPRESENTATION(#178,#13973);
#273=CONTEXT_DEPENDENT_SHAPE_REPRESENTATION(#179,#13974);
#274=CONTEXT_DEPENDENT_SHAPE_REPRESENTATION(#180,#13975);
#275=CONTEXT_DEPENDENT_SHAPE_REPRESENTATION(#181,#13976);
#276=CONTEXT_DEPENDENT_SHAPE_REPRESENTATION(#182,#13977);
#277=CONTEXT_DEPENDENT_SHAPE_REPRESENTATION(#183,#13978);
#278=CONTEXT_DEPENDENT_SHAPE_REPRESENTATION(#184,#13979);
#279=CONTEXT_DEPENDENT_SHAPE_REPRESENTATION(#185,#13980);
#280=CONTEXT_DEPENDENT_SHAPE_REPRESENTATION(#186,#13981);
#281=CONTEXT_DEPENDENT_SHAPE_REPRESENTATION(#187,#13982);
#282=CONTEXT_DEPENDENT_SHAPE_REPRESENTATION(#188,#13983);
#283=CONTEXT_DEPENDENT_SHAPE_REPRESENTATION(#189,#13984);
#284=CONTEXT_DEPENDENT_SHAPE_REPRESENTATION(#190,#13985);
#285=CONTEXT_DEPENDENT_SHAPE_REPRESENTATION(#191,#13986);
#286=CONTEXT_DEPENDENT_SHAPE_REPRESENTATION(#192,#13987);
#287=CONTEXT_DEPENDENT_SHAPE_REPRESENTATION(#193,#13988);
#288=CONTEXT_DEPENDENT_SHAPE_REPRESENTATION(#194,#13989);
#289=CONTEXT_DEPENDENT_SHAPE_REPRESENTATION(#195,#13990);
#290=CONTEXT_DEPENDENT_SHAPE_REPRESENTATION(#196,#13991);
#291=CONTEXT_DEPENDENT_SHAPE_REPRESENTATION(#197,#13992);
#292=CONTEXT_DEPENDENT_SHAPE_REPRESENTATION(#198,#13993);
#293=CONTEXT_DEPENDENT_SHAPE_REPRESENTATION(#199,#13994);
#294=CONTEXT_DEPENDENT_SHAPE_REPRESENTATION(#200,#13995);
#295=NEXT_ASSEMBLY_USAGE_OCCURRENCE('Inner ring:1','Inner ring:1',
'Inner ring:1',#14061,#14062,'Inner ring:1');
#296=NEXT_ASSEMBLY_USAGE_OCCURRENCE('Outer ring:1','Outer ring:1',
'Outer ring:1',#14061,#14063,'Outer ring:1');
#297=NEXT_ASSEMBLY_USAGE_OCCURRENCE('Balls:1','Balls:1','Balls:1',#14061,
#14064,'Balls:1');
#298=NEXT_ASSEMBLY_USAGE_OCCURRENCE('Cage:1','Cage:1','Cage:1',#14061,#14065,
'Cage:1');
#299=NEXT_ASSEMBLY_USAGE_OCCURRENCE('Seals 2RS:1','Seals 2RS:1',
'Seals 2RS:1',#14061,#14066,'Seals 2RS:1');
#300=NEXT_ASSEMBLY_USAGE_OCCURRENCE('Drilled 400 mm rail:2',
'Drilled 400 mm rail:2','Drilled 400 mm rail:2',#14036,#14038,
'Drilled 400 mm rail:2');
#301=NEXT_ASSEMBLY_USAGE_OCCURRENCE('Drilled 200 mm rail:2',
'Drilled 200 mm rail:2','Drilled 200 mm rail:2',#14036,#14039,
'Drilled 200 mm rail:2');
#302=NEXT_ASSEMBLY_USAGE_OCCURRENCE(
'Slotted Extrusion - 20 x 20 x 200 mm:2',
'Slotted Extrusion - 20 x 20 x 200 mm:2',
'Slotted Extrusion - 20 x 20 x 200 mm:2',#14036,#14040,
'Slotted Extrusion - 20 x 20 x 200 mm:2');
#303=NEXT_ASSEMBLY_USAGE_OCCURRENCE('Flat Washer - M5:2',
'Flat Washer - M5:2','Flat Washer - M5:2',#14036,#14044,
'Flat Washer - M5:2');
#304=NEXT_ASSEMBLY_USAGE_OCCURRENCE('M5x40 leg screw:2',
'M5x40 leg screw:2','M5x40 leg screw:2',#14036,#14041,
'M5x40 leg screw:2');
#305=NEXT_ASSEMBLY_USAGE_OCCURRENCE('Flat Washer - M5:3',
'Flat Washer - M5:3','Flat Washer - M5:3',#14036,#14044,
'Flat Washer - M5:3');
#306=NEXT_ASSEMBLY_USAGE_OCCURRENCE('Cap Screw - M5x20:2',
'Cap Screw - M5x20:2','Cap Screw - M5x20:2',#14036,#14042,
'Cap Screw - M5x20:2');
#307=NEXT_ASSEMBLY_USAGE_OCCURRENCE(
'Slotted Extrusion - 20 x 20 x 200 mm:3',
'Slotted Extrusion - 20 x 20 x 200 mm:3',
'Slotted Extrusion - 20 x 20 x 200 mm:3',#14036,#14040,
'Slotted Extrusion - 20 x 20 x 200 mm:3');
#308=NEXT_ASSEMBLY_USAGE_OCCURRENCE('Flat Washer - M5:4',
'Flat Washer - M5:4','Flat Washer - M5:4',#14036,#14044,
'Flat Washer - M5:4');
#309=NEXT_ASSEMBLY_USAGE_OCCURRENCE('M5x40 leg screw:3',
'M5x40 leg screw:3','M5x40 leg screw:3',#14036,#14041,
'M5x40 leg screw:3');
#310=NEXT_ASSEMBLY_USAGE_OCCURRENCE('Flat Washer - M5:5',
'Flat Washer - M5:5','Flat Washer - M5:5',#14036,#14044,
'Flat Washer - M5:5');
#311=NEXT_ASSEMBLY_USAGE_OCCURRENCE('Cap Screw - M5x20:3',
'Cap Screw - M5x20:3','Cap Screw - M5x20:3',#14036,#14042,
'Cap Screw - M5x20:3');
#312=NEXT_ASSEMBLY_USAGE_OCCURRENCE('Rail splice plate:1',
'Rail splice plate:1','Rail splice plate:1',#14036,#14037,
'Rail splice plate:1');
#313=NEXT_ASSEMBLY_USAGE_OCCURRENCE('Captive slot nut:2',
'Captive slot nut:2','Captive slot nut:2',#14036,#14070,
'Captive slot nut:2');
#314=NEXT_ASSEMBLY_USAGE_OCCURRENCE('Flat Washer - M5:6',
'Flat Washer - M5:6','Flat Washer - M5:6',#14036,#14044,
'Flat Washer - M5:6');
#315=NEXT_ASSEMBLY_USAGE_OCCURRENCE('M5x14 Cap Screw:2',
'M5x14 Cap Screw:2','M5x14 Cap Screw:2',#14036,#14071,
'M5x14 Cap Screw:2');
#316=NEXT_ASSEMBLY_USAGE_OCCURRENCE('Captive slot nut:3',
'Captive slot nut:3','Captive slot nut:3',#14036,#14070,
'Captive slot nut:3');
#317=NEXT_ASSEMBLY_USAGE_OCCURRENCE('Flat Washer - M5:7',
'Flat Washer - M5:7','Flat Washer - M5:7',#14036,#14044,
'Flat Washer - M5:7');
#318=NEXT_ASSEMBLY_USAGE_OCCURRENCE('M5x14 Cap Screw:3',
'M5x14 Cap Screw:3','M5x14 Cap Screw:3',#14036,#14071,
'M5x14 Cap Screw:3');
#319=NEXT_ASSEMBLY_USAGE_OCCURRENCE('Captive slot nut:4',
'Captive slot nut:4','Captive slot nut:4',#14036,#14070,
'Captive slot nut:4');
#320=NEXT_ASSEMBLY_USAGE_OCCURRENCE('Flat Washer - M5:8',
'Flat Washer - M5:8','Flat Washer - M5:8',#14036,#14044,
'Flat Washer - M5:8');
#321=NEXT_ASSEMBLY_USAGE_OCCURRENCE('M5x14 Cap Screw:4',
'M5x14 Cap Screw:4','M5x14 Cap Screw:4',#14036,#14071,
'M5x14 Cap Screw:4');
#322=NEXT_ASSEMBLY_USAGE_OCCURRENCE('Captive slot nut:5',
'Captive slot nut:5','Captive slot nut:5',#14036,#14070,
'Captive slot nut:5');
#323=NEXT_ASSEMBLY_USAGE_OCCURRENCE('Flat Washer - M5:9',
'Flat Washer - M5:9','Flat Washer - M5:9',#14036,#14044,
'Flat Washer - M5:9');
#324=NEXT_ASSEMBLY_USAGE_OCCURRENCE('M5x14 Cap Screw:5',
'M5x14 Cap Screw:5','M5x14 Cap Screw:5',#14036,#14071,
'M5x14 Cap Screw:5');
#325=NEXT_ASSEMBLY_USAGE_OCCURRENCE('Drilled 400 mm rail:3',
'Drilled 400 mm rail:3','Drilled 400 mm rail:3',#14036,#14038,
'Drilled 400 mm rail:3');
#326=NEXT_ASSEMBLY_USAGE_OCCURRENCE('Drilled 200 mm rail:3',
'Drilled 200 mm rail:3','Drilled 200 mm rail:3',#14036,#14039,
'Drilled 200 mm rail:3');
#327=NEXT_ASSEMBLY_USAGE_OCCURRENCE(
'Slotted Extrusion - 20 x 20 x 200 mm:4',
'Slotted Extrusion - 20 x 20 x 200 mm:4',
'Slotted Extrusion - 20 x 20 x 200 mm:4',#14036,#14040,
'Slotted Extrusion - 20 x 20 x 200 mm:4');
#328=NEXT_ASSEMBLY_USAGE_OCCURRENCE('Flat Washer - M5:10',
'Flat Washer - M5:10','Flat Washer - M5:10',#14036,#14044,
'Flat Washer - M5:10');
#329=NEXT_ASSEMBLY_USAGE_OCCURRENCE('M5x40 leg screw:4',
'M5x40 leg screw:4','M5x40 leg screw:4',#14036,#14041,
'M5x40 leg screw:4');
#330=NEXT_ASSEMBLY_USAGE_OCCURRENCE('Flat Washer - M5:11',
'Flat Washer - M5:11','Flat Washer - M5:11',#14036,#14044,
'Flat Washer - M5:11');
#331=NEXT_ASSEMBLY_USAGE_OCCURRENCE('Cap Screw - M5x20:4',
'Cap Screw - M5x20:4','Cap Screw - M5x20:4',#14036,#14042,
'Cap Screw - M5x20:4');
#332=NEXT_ASSEMBLY_USAGE_OCCURRENCE(
'Slotted Extrusion - 20 x 20 x 200 mm:5',
'Slotted Extrusion - 20 x 20 x 200 mm:5',
'Slotted Extrusion - 20 x 20 x 200 mm:5',#14036,#14040,
'Slotted Extrusion - 20 x 20 x 200 mm:5');
#333=NEXT_ASSEMBLY_USAGE_OCCURRENCE('Flat Washer - M5:12',
'Flat Washer - M5:12','Flat Washer - M5:12',#14036,#14044,
'Flat Washer - M5:12');
#334=NEXT_ASSEMBLY_USAGE_OCCURRENCE('M5x40 leg screw:5',
'M5x40 leg screw:5','M5x40 leg screw:5',#14036,#14041,
'M5x40 leg screw:5');
#335=NEXT_ASSEMBLY_USAGE_OCCURRENCE('Flat Washer - M5:13',
'Flat Washer - M5:13','Flat Washer - M5:13',#14036,#14044,
'Flat Washer - M5:13');
#336=NEXT_ASSEMBLY_USAGE_OCCURRENCE('Cap Screw - M5x20:5',
'Cap Screw - M5x20:5','Cap Screw - M5x20:5',#14036,#14042,
'Cap Screw - M5x20:5');
#337=NEXT_ASSEMBLY_USAGE_OCCURRENCE('Rail splice plate (1):1',
'Rail splice plate (1):1','Rail splice plate (1):1',#14036,#14043,
'Rail splice plate (1):1');
#338=NEXT_ASSEMBLY_USAGE_OCCURRENCE('Captive slot nut:6',
'Captive slot nut:6','Captive slot nut:6',#14036,#14070,
'Captive slot nut:6');
#339=NEXT_ASSEMBLY_USAGE_OCCURRENCE('Flat Washer - M5:14',
'Flat Washer - M5:14','Flat Washer - M5:14',#14036,#14044,
'Flat Washer - M5:14');
#340=NEXT_ASSEMBLY_USAGE_OCCURRENCE('M5x14 Cap Screw:6',
'M5x14 Cap Screw:6','M5x14 Cap Screw:6',#14036,#14071,
'M5x14 Cap Screw:6');
#341=NEXT_ASSEMBLY_USAGE_OCCURRENCE('Captive slot nut:7',
'Captive slot nut:7','Captive slot nut:7',#14036,#14070,
'Captive slot nut:7');
#342=NEXT_ASSEMBLY_USAGE_OCCURRENCE('Flat Washer - M5:15',
'Flat Washer - M5:15','Flat Washer - M5:15',#14036,#14044,
'Flat Washer - M5:15');
#343=NEXT_ASSEMBLY_USAGE_OCCURRENCE('M5x14 Cap Screw:7',
'M5x14 Cap Screw:7','M5x14 Cap Screw:7',#14036,#14071,
'M5x14 Cap Screw:7');
#344=NEXT_ASSEMBLY_USAGE_OCCURRENCE('Captive slot nut:8',
'Captive slot nut:8','Captive slot nut:8',#14036,#14070,
'Captive slot nut:8');
#345=NEXT_ASSEMBLY_USAGE_OCCURRENCE('Flat Washer - M5:16',
'Flat Washer - M5:16','Flat Washer - M5:16',#14036,#14044,
'Flat Washer - M5:16');
#346=NEXT_ASSEMBLY_USAGE_OCCURRENCE('M5x14 Cap Screw:8',
'M5x14 Cap Screw:8','M5x14 Cap Screw:8',#14036,#14071,
'M5x14 Cap Screw:8');
#347=NEXT_ASSEMBLY_USAGE_OCCURRENCE('Captive slot nut:9',
'Captive slot nut:9','Captive slot nut:9',#14036,#14070,
'Captive slot nut:9');
#348=NEXT_ASSEMBLY_USAGE_OCCURRENCE('Flat Washer - M5:17',
'Flat Washer - M5:17','Flat Washer - M5:17',#14036,#14044,
'Flat Washer - M5:17');
#349=NEXT_ASSEMBLY_USAGE_OCCURRENCE('M5x14 Cap Screw:9',
'M5x14 Cap Screw:9','M5x14 Cap Screw:9',#14036,#14071,
'M5x14 Cap Screw:9');
#350=NEXT_ASSEMBLY_USAGE_OCCURRENCE('Cross foot:1','Cross foot:1',
'Cross foot:1',#14036,#14045,'Cross foot:1');
#351=NEXT_ASSEMBLY_USAGE_OCCURRENCE('Bonded foot pad:1',
'Bonded foot pad:1','Bonded foot pad:1',#14036,#14046,
'Bonded foot pad:1');
#352=NEXT_ASSEMBLY_USAGE_OCCURRENCE('Bonded foot pad (1):1',
'Bonded foot pad (1):1','Bonded foot pad (1):1',#14036,#14047,
'Bonded foot pad (1):1');
#353=NEXT_ASSEMBLY_USAGE_OCCURRENCE('Cross foot (1):1',
'Cross foot (1):1','Cross foot (1):1',#14036,#14048,'Cross foot (1):1');
#354=NEXT_ASSEMBLY_USAGE_OCCURRENCE('Bonded foot pad (2):1',
'Bonded foot pad (2):1','Bonded foot pad (2):1',#14036,#14049,
'Bonded foot pad (2):1');
#355=NEXT_ASSEMBLY_USAGE_OCCURRENCE('Bonded foot pad (3):1',
'Bonded foot pad (3):1','Bonded foot pad (3):1',#14036,#14050,
'Bonded foot pad (3):1');
#356=NEXT_ASSEMBLY_USAGE_OCCURRENCE('Roller tube:1','Roller tube:1',
'Roller tube:1',#14051,#14052,'Roller tube:1');
#357=NEXT_ASSEMBLY_USAGE_OCCURRENCE('Bearing insert:1',
'Bearing insert:1','Bearing insert:1',#14051,#14053,'Bearing insert:1');
#358=NEXT_ASSEMBLY_USAGE_OCCURRENCE('Bearing retainer:1',
'Bearing retainer:1','Bearing retainer:1',#14051,#14054,
'Bearing retainer:1');
#359=NEXT_ASSEMBLY_USAGE_OCCURRENCE('Bearing insert (1):1',
'Bearing insert (1):1','Bearing insert (1):1',#14051,#14055,
'Bearing insert (1):1');
#360=NEXT_ASSEMBLY_USAGE_OCCURRENCE('Bearing retainer (1):1',
'Bearing retainer (1):1','Bearing retainer (1):1',#14051,#14056,
'Bearing retainer (1):1');
#361=NEXT_ASSEMBLY_USAGE_OCCURRENCE('Dead axle:1','Dead axle:1',
'Dead axle:1',#14051,#14057,'Dead axle:1');
#362=NEXT_ASSEMBLY_USAGE_OCCURRENCE('Axle support:1','Axle support:1',
'Axle support:1',#14051,#14058,'Axle support:1');
#363=NEXT_ASSEMBLY_USAGE_OCCURRENCE('Axle keeper:1','Axle keeper:1',
'Axle keeper:1',#14051,#14059,'Axle keeper:1');
#364=NEXT_ASSEMBLY_USAGE_OCCURRENCE('Inner race spacer:1',
'Inner race spacer:1','Inner race spacer:1',#14051,#14060,
'Inner race spacer:1');
#365=NEXT_ASSEMBLY_USAGE_OCCURRENCE(
'Sealed Ball Bearing - 10 x 30 x 9 mm:2',
'Sealed Ball Bearing - 10 x 30 x 9 mm:2',
'Sealed Ball Bearing - 10 x 30 x 9 mm:2',#14051,#14061,
'Sealed Ball Bearing - 10 x 30 x 9 mm:2');
#366=NEXT_ASSEMBLY_USAGE_OCCURRENCE('M4x10 Cap Screw:2',
'M4x10 Cap Screw:2','M4x10 Cap Screw:2',#14051,#14068,
'M4x10 Cap Screw:2');
#367=NEXT_ASSEMBLY_USAGE_OCCURRENCE('Captive slot nut:11',
'Captive slot nut:11','Captive slot nut:11',#14051,#14070,
'Captive slot nut:11');
#368=NEXT_ASSEMBLY_USAGE_OCCURRENCE('M5x14 Cap Screw:11',
'M5x14 Cap Screw:11','M5x14 Cap Screw:11',#14051,#14071,
'M5x14 Cap Screw:11');
#369=NEXT_ASSEMBLY_USAGE_OCCURRENCE('M5x14 Cap Screw:10',
'M5x14 Cap Screw:10','M5x14 Cap Screw:10',#14051,#14071,
'M5x14 Cap Screw:10');
#370=NEXT_ASSEMBLY_USAGE_OCCURRENCE('Captive slot nut:10',
'Captive slot nut:10','Captive slot nut:10',#14051,#14070,
'Captive slot nut:10');
#371=NEXT_ASSEMBLY_USAGE_OCCURRENCE(
'Sealed Ball Bearing - 10 x 30 x 9 mm:3',
'Sealed Ball Bearing - 10 x 30 x 9 mm:3',
'Sealed Ball Bearing - 10 x 30 x 9 mm:3',#14051,#14061,
'Sealed Ball Bearing - 10 x 30 x 9 mm:3');
#372=NEXT_ASSEMBLY_USAGE_OCCURRENCE('Inner race spacer (1):1',
'Inner race spacer (1):1','Inner race spacer (1):1',#14051,#14067,
'Inner race spacer (1):1');
#373=NEXT_ASSEMBLY_USAGE_OCCURRENCE('M4x10 Cap Screw:3',
'M4x10 Cap Screw:3','M4x10 Cap Screw:3',#14051,#14068,
'M4x10 Cap Screw:3');
#374=NEXT_ASSEMBLY_USAGE_OCCURRENCE('Axle keeper (1):1',
'Axle keeper (1):1','Axle keeper (1):1',#14051,#14069,
'Axle keeper (1):1');
#375=NEXT_ASSEMBLY_USAGE_OCCURRENCE('Captive slot nut:13',
'Captive slot nut:13','Captive slot nut:13',#14051,#14070,
'Captive slot nut:13');
#376=NEXT_ASSEMBLY_USAGE_OCCURRENCE('M5x14 Cap Screw:12',
'M5x14 Cap Screw:12','M5x14 Cap Screw:12',#14051,#14071,
'M5x14 Cap Screw:12');
#377=NEXT_ASSEMBLY_USAGE_OCCURRENCE('Captive slot nut:12',
'Captive slot nut:12','Captive slot nut:12',#14051,#14070,
'Captive slot nut:12');
#378=NEXT_ASSEMBLY_USAGE_OCCURRENCE('M5x14 Cap Screw:13',
'M5x14 Cap Screw:13','M5x14 Cap Screw:13',#14051,#14071,
'M5x14 Cap Screw:13');
#379=NEXT_ASSEMBLY_USAGE_OCCURRENCE('Axle support (1):1',
'Axle support (1):1','Axle support (1):1',#14051,#14072,
'Axle support (1):1');
#380=NEXT_ASSEMBLY_USAGE_OCCURRENCE('Conveyor frame:1',
'Conveyor frame:1','Conveyor frame:1',#14035,#14036,'Conveyor frame:1');
#381=NEXT_ASSEMBLY_USAGE_OCCURRENCE('Roller 1:1','Roller 1:1',
'Roller 1:1',#14035,#14051,'Roller 1:1');
#382=NEXT_ASSEMBLY_USAGE_OCCURRENCE('Roller 1:2','Roller 1:2',
'Roller 1:2',#14035,#14051,'Roller 1:2');
#383=NEXT_ASSEMBLY_USAGE_OCCURRENCE('Roller 1:3','Roller 1:3',
'Roller 1:3',#14035,#14051,'Roller 1:3');
#384=NEXT_ASSEMBLY_USAGE_OCCURRENCE('Roller 1:4','Roller 1:4',
'Roller 1:4',#14035,#14051,'Roller 1:4');
#385=NEXT_ASSEMBLY_USAGE_OCCURRENCE('Roller 1:5','Roller 1:5',
'Roller 1:5',#14035,#14051,'Roller 1:5');
#386=NEXT_ASSEMBLY_USAGE_OCCURRENCE('Roller 1:6','Roller 1:6',
'Roller 1:6',#14035,#14051,'Roller 1:6');
#387=NEXT_ASSEMBLY_USAGE_OCCURRENCE('Roller 1:7','Roller 1:7',
'Roller 1:7',#14035,#14051,'Roller 1:7');
#388=NEXT_ASSEMBLY_USAGE_OCCURRENCE('Roller 1:8','Roller 1:8',
'Roller 1:8',#14035,#14051,'Roller 1:8');
#389=SPHERICAL_SURFACE('',#8525,0.23815);
#390=SPHERICAL_SURFACE('',#8527,0.23815);
#391=SPHERICAL_SURFACE('',#8529,0.23815);
#392=SPHERICAL_SURFACE('',#8531,0.23815);
#393=SPHERICAL_SURFACE('',#8533,0.23815);
#394=SPHERICAL_SURFACE('',#8535,0.23815);
#395=SPHERICAL_SURFACE('',#8537,0.23815);
#396=SPHERICAL_SURFACE('',#8539,0.23815);
#397=SPHERICAL_SURFACE('',#8542,0.247676);
#398=SPHERICAL_SURFACE('',#8558,0.247676);
#399=SPHERICAL_SURFACE('',#8563,0.247676);
#400=SPHERICAL_SURFACE('',#8568,0.247676);
#401=SPHERICAL_SURFACE('',#8573,0.247676);
#402=SPHERICAL_SURFACE('',#8578,0.247676);
#403=SPHERICAL_SURFACE('',#8583,0.247676);
#404=SPHERICAL_SURFACE('',#8591,0.247676);
#405=TOROIDAL_SURFACE('',#8485,1.,0.247676);
#406=TOROIDAL_SURFACE('',#8505,1.,0.247676);
#407=CONICAL_SURFACE('',#8244,0.4,0.785398163397448);
#408=CONICAL_SURFACE('',#8248,0.41,0.785398163397448);
#409=CONICAL_SURFACE('',#8252,0.26,0.463647609000806);
#410=CONICAL_SURFACE('',#8258,0.4,0.785398163397448);
#411=CONICAL_SURFACE('',#8262,0.41,0.785398163397448);
#412=CONICAL_SURFACE('',#8266,0.26,0.463647609000806);
#413=CONICAL_SURFACE('',#8270,0.225,0.785398163397448);
#414=CONICAL_SURFACE('',#8301,0.275,0.785398163397449);
#415=CONICAL_SURFACE('',#8496,0.53,0.785398163397448);
#416=CONICAL_SURFACE('',#8503,0.53,0.785398163397448);
#417=CONICAL_SURFACE('',#8516,1.47,0.785398163397449);
#418=CONICAL_SURFACE('',#8520,1.47,0.785398163397449);
#419=CONICAL_SURFACE('',#8639,0.325,0.785398163397448);
#420=CONICAL_SURFACE('',#8643,0.335,0.785398163397448);
#421=CONICAL_SURFACE('',#8647,0.21,0.463647609000806);
#422=CONICAL_SURFACE('',#8693,0.4,0.785398163397448);
#423=CONICAL_SURFACE('',#8697,0.41,0.785398163397448);
#424=CONICAL_SURFACE('',#8701,0.26,0.463647609000806);
#425=ORIENTED_CLOSED_SHELL('',*,#7631,.F.);
#426=ORIENTED_CLOSED_SHELL('',*,#7634,.F.);
#427=ORIENTED_CLOSED_SHELL('',*,#7666,.F.);
#428=ORIENTED_CLOSED_SHELL('',*,#7670,.F.);
#429=BREP_WITH_VOIDS('Body1',#7632,(#425));
#430=BREP_WITH_VOIDS('Body1',#7633,(#426));
#431=BREP_WITH_VOIDS('Body1',#7667,(#427));
#432=BREP_WITH_VOIDS('Body1',#7671,(#428));
#433=B_SPLINE_CURVE_WITH_KNOTS('',3,(#11133,#11134,#11135,#11136,#11137,
#11138,#11139,#11140,#11141,#11142,#11143,#11144,#11145,#11146,#11147,#11148,
#11149,#11150,#11151,#11152,#11153,#11154),.UNSPECIFIED.,.F.,.F.,(4,2,2,
2,2,2,2,2,2,2,4),(0.335938049981194,0.418928967949028,0.501919885916861,
0.586897992939625,0.629387046451007,0.671876099962389,0.714365153473771,
0.756854206985153,0.841832314007917,0.92482323197575,1.00781414994358),
 .UNSPECIFIED.);
#434=B_SPLINE_CURVE_WITH_KNOTS('',3,(#11159,#11160,#11161,#11162,#11163,
#11164,#11165,#11166,#11167,#11168,#11169,#11170),.UNSPECIFIED.,.F.,.F.,
(4,2,2,2,2,4),(0.,0.0424890535113821,0.0849781070227642,0.169956214045528,
0.252947132013361,0.335938049981194),.UNSPECIFIED.);
#435=B_SPLINE_CURVE_WITH_KNOTS('',3,(#11171,#11172,#11173,#11174,#11175,
#11176,#11177,#11178,#11179,#11180,#11181,#11182),.UNSPECIFIED.,.F.,.F.,
(4,2,2,2,2,4),(1.00781414994358,1.09080506791142,1.17379598587925,1.25877409290201,
1.3012631464134,1.34375219992478),.UNSPECIFIED.);
#436=B_SPLINE_CURVE_WITH_KNOTS('',3,(#11185,#11186,#11187,#11188,#11189,
#11190,#11191,#11192,#11193,#11194,#11195,#11196,#11197,#11198,#11199,#11200,
#11201,#11202,#11203,#11204,#11205,#11206,#11207,#11208,#11209,#11210,#11211,
#11212,#11213,#11214,#11215,#11216),.UNSPECIFIED.,.F.,.F.,(4,2,2,2,2,2,
2,2,2,2,2,2,2,2,2,4),(0.,0.0424890535113822,0.0849781070227643,0.169956214045529,
0.252947132013362,0.335938049981195,0.418928967949028,0.501919885916861,
0.586897992939625,0.629387046451007,0.671876099962389,0.714365153473771,
0.756854206985153,0.841832314007917,0.924823231975751,1.00781414994358),
 .UNSPECIFIED.);
#437=B_SPLINE_CURVE_WITH_KNOTS('',3,(#11217,#11218,#11219,#11220,#11221,
#11222,#11223,#11224,#11225,#11226,#11227,#11228),.UNSPECIFIED.,.F.,.F.,
(4,2,2,2,2,4),(1.00781414994358,1.09080506791142,1.17379598587925,1.25877409290201,
1.3012631464134,1.34375219992478),.UNSPECIFIED.);
#438=B_SPLINE_CURVE_WITH_KNOTS('',3,(#11510,#11511,#11512,#11513,#11514,
#11515,#11516,#11517,#11518,#11519,#11520,#11521,#11522,#11523,#11524,#11525,
#11526,#11527,#11528,#11529,#11530,#11531),.UNSPECIFIED.,.F.,.F.,(4,2,2,
2,2,2,2,2,2,2,4),(0.335938049981195,0.418928967949028,0.501919885916861,
0.586897992939625,0.629387046451008,0.67187609996239,0.714365153473772,
0.756854206985154,0.841832314007919,0.924823231975752,1.00781414994358),
 .UNSPECIFIED.);
#439=B_SPLINE_CURVE_WITH_KNOTS('',3,(#11536,#11537,#11538,#11539,#11540,
#11541,#11542,#11543,#11544,#11545,#11546,#11547),.UNSPECIFIED.,.F.,.F.,
(4,2,2,2,2,4),(0.,0.0424890535113822,0.0849781070227644,0.169956214045529,
0.252947132013362,0.335938049981195),.UNSPECIFIED.);
#440=B_SPLINE_CURVE_WITH_KNOTS('',3,(#11548,#11549,#11550,#11551,#11552,
#11553,#11554,#11555,#11556,#11557,#11558,#11559),.UNSPECIFIED.,.F.,.F.,
(4,2,2,2,2,4),(1.00781414994358,1.09080506791142,1.17379598587925,1.25877409290202,
1.3012631464134,1.34375219992478),.UNSPECIFIED.);
#441=B_SPLINE_CURVE_WITH_KNOTS('',3,(#11562,#11563,#11564,#11565,#11566,
#11567,#11568,#11569,#11570,#11571,#11572,#11573,#11574,#11575,#11576,#11577,
#11578,#11579,#11580,#11581,#11582,#11583,#11584,#11585,#11586,#11587,#11588,
#11589,#11590,#11591,#11592,#11593),.UNSPECIFIED.,.F.,.F.,(4,2,2,2,2,2,
2,2,2,2,2,2,2,2,2,4),(0.,0.0424890535113822,0.0849781070227644,0.169956214045529,
0.252947132013362,0.335938049981195,0.418928967949028,0.501919885916861,
0.586897992939625,0.629387046451008,0.67187609996239,0.714365153473772,
0.756854206985154,0.841832314007919,0.924823231975752,1.00781414994358),
 .UNSPECIFIED.);
#442=B_SPLINE_CURVE_WITH_KNOTS('',3,(#11594,#11595,#11596,#11597,#11598,
#11599,#11600,#11601,#11602,#11603,#11604,#11605),.UNSPECIFIED.,.F.,.F.,
(4,2,2,2,2,4),(1.00781414994358,1.09080506791142,1.17379598587925,1.25877409290202,
1.3012631464134,1.34375219992478),.UNSPECIFIED.);
#443=B_SPLINE_CURVE_WITH_KNOTS('',3,(#12876,#12877,#12878,#12879,#12880,
#12881,#12882,#12883,#12884,#12885,#12886,#12887,#12888,#12889,#12890,#12891,
#12892,#12893,#12894,#12895,#12896,#12897),.UNSPECIFIED.,.F.,.F.,(4,2,2,
2,2,2,2,2,2,2,4),(0.0473477652366656,0.126350602536658,0.189525903804987,
0.252701205073317,0.313298422430275,0.373895639787233,0.434492857144191,
0.495090074501149,0.558265375769478,0.621440677037807,0.7004435143378),
 .UNSPECIFIED.);
#444=B_SPLINE_CURVE_WITH_KNOTS('',3,(#12901,#12902,#12903,#12904,#12905,
#12906,#12907,#12908,#12909,#12910,#12911,#12912,#12913,#12914,#12915,#12916,
#12917,#12918,#12919,#12920,#12921,#12922),.UNSPECIFIED.,.F.,.F.,(4,2,2,
2,2,2,2,2,2,2,4),(0.0464897534940957,0.0852567806515119,0.170513561303024,
0.246687263103517,0.308657850341199,0.370628437578881,0.432599024816563,
0.494569612054245,0.570743313854739,0.656000094506251,0.694767121663666),
 .UNSPECIFIED.);
#445=B_SPLINE_CURVE_WITH_KNOTS('',3,(#12928,#12929,#12930,#12931,#12932,
#12933,#12934,#12935,#12936,#12937,#12938,#12939,#12940,#12941,#12942,#12943,
#12944,#12945,#12946,#12947,#12948,#12949),.UNSPECIFIED.,.F.,.F.,(4,2,2,
2,2,2,2,2,2,2,4),(0.0464897534940957,0.0852567806515118,0.170513561303024,
0.246687263103517,0.308657850341199,0.370628437578881,0.432599024816563,
0.494569612054245,0.570743313854738,0.65600009450625,0.694767121663666),
 .UNSPECIFIED.);
#446=B_SPLINE_CURVE_WITH_KNOTS('',3,(#12953,#12954,#12955,#12956,#12957,
#12958,#12959,#12960,#12961,#12962,#12963,#12964,#12965,#12966,#12967,#12968,
#12969,#12970,#12971,#12972,#12973,#12974),.UNSPECIFIED.,.F.,.F.,(4,2,2,
2,2,2,2,2,2,2,4),(0.0464897534940957,0.0852567806515119,0.170513561303024,
0.246687263103517,0.308657850341199,0.370628437578881,0.432599024816563,
0.494569612054245,0.570743313854739,0.656000094506251,0.694767121663666),
 .UNSPECIFIED.);
#447=B_SPLINE_CURVE_WITH_KNOTS('',3,(#12978,#12979,#12980,#12981,#12982,
#12983,#12984,#12985,#12986,#12987,#12988,#12989),.UNSPECIFIED.,.F.,.F.,
(4,2,2,2,2,4),(0.0464897534940957,0.0852567806515119,0.170513561303024,
0.246687263103517,0.308657850341199,0.370628437578881),.UNSPECIFIED.);
#448=B_SPLINE_CURVE_WITH_KNOTS('',3,(#12994,#12995,#12996,#12997,#12998,
#12999,#13000,#13001,#13002,#13003,#13004,#13005),.UNSPECIFIED.,.F.,.F.,
(4,2,2,2,2,4),(0.370628437578881,0.432599024816563,0.494569612054245,0.570743313854738,
0.65600009450625,0.694767121663666),.UNSPECIFIED.);
#449=B_SPLINE_CURVE_WITH_KNOTS('',3,(#13009,#13010,#13011,#13012,#13013,
#13014,#13015,#13016,#13017,#13018,#13019,#13020,#13021,#13022,#13023,#13024,
#13025,#13026,#13027,#13028,#13029,#13030),.UNSPECIFIED.,.F.,.F.,(4,2,2,
2,2,2,2,2,2,2,4),(0.0464897534940957,0.0852567806515121,0.170513561303024,
0.246687263103518,0.308657850341199,0.370628437578881,0.432599024816563,
0.494569612054245,0.570743313854738,0.65600009450625,0.694767121663666),
 .UNSPECIFIED.);
#450=B_SPLINE_CURVE_WITH_KNOTS('',3,(#13034,#13035,#13036,#13037,#13038,
#13039,#13040,#13041,#13042,#13043,#13044,#13045,#13046,#13047,#13048,#13049,
#13050,#13051,#13052,#13053,#13054,#13055),.UNSPECIFIED.,.F.,.F.,(4,2,2,
2,2,2,2,2,2,2,4),(0.0464897534940957,0.0852567806515119,0.170513561303024,
0.246687263103517,0.308657850341199,0.370628437578881,0.432599024816563,
0.494569612054245,0.570743313854738,0.65600009450625,0.694767121663667),
 .UNSPECIFIED.);
#451=B_SPLINE_CURVE_WITH_KNOTS('',3,(#13059,#13060,#13061,#13062,#13063,
#13064,#13065,#13066,#13067,#13068,#13069,#13070,#13071,#13072,#13073,#13074,
#13075,#13076,#13077,#13078,#13079,#13080),.UNSPECIFIED.,.F.,.F.,(4,2,2,
2,2,2,2,2,2,2,4),(0.0464897534940957,0.0852567806515119,0.170513561303024,
0.246687263103517,0.308657850341199,0.370628437578881,0.432599024816563,
0.494569612054245,0.570743313854738,0.65600009450625,0.694767121663666),
 .UNSPECIFIED.);
#452=B_SPLINE_CURVE_WITH_KNOTS('',3,(#13084,#13085,#13086,#13087,#13088,
#13089,#13090,#13091,#13092,#13093,#13094,#13095,#13096,#13097,#13098,#13099,
#13100,#13101,#13102,#13103,#13104,#13105),.UNSPECIFIED.,.F.,.F.,(4,2,2,
2,2,2,2,2,2,2,4),(0.0464897534940957,0.0852567806515119,0.170513561303024,
0.246687263103517,0.308657850341199,0.370628437578881,0.432599024816563,
0.494569612054245,0.570743313854739,0.656000094506251,0.694767121663667),
 .UNSPECIFIED.);
#453=B_SPLINE_CURVE_WITH_KNOTS('',3,(#13113,#13114,#13115,#13116,#13117,
#13118,#13119,#13120,#13121,#13122,#13123,#13124,#13125,#13126,#13127,#13128,
#13129,#13130,#13131,#13132,#13133,#13134),.UNSPECIFIED.,.F.,.F.,(4,2,2,
2,2,2,2,2,2,2,4),(0.0473477652366656,0.126350602536658,0.189525903804987,
0.252701205073316,0.313298422430274,0.373895639787232,0.434492857144191,
0.495090074501149,0.558265375769478,0.621440677037807,0.7004435143378),
 .UNSPECIFIED.);
#454=B_SPLINE_CURVE_WITH_KNOTS('',3,(#13142,#13143,#13144,#13145,#13146,
#13147,#13148,#13149,#13150,#13151,#13152,#13153,#13154,#13155,#13156,#13157,
#13158,#13159,#13160,#13161,#13162,#13163),.UNSPECIFIED.,.F.,.F.,(4,2,2,
2,2,2,2,2,2,2,4),(0.0473477652366656,0.126350602536658,0.189525903804987,
0.252701205073317,0.313298422430275,0.373895639787233,0.434492857144191,
0.495090074501149,0.558265375769478,0.621440677037807,0.7004435143378),
 .UNSPECIFIED.);
#455=B_SPLINE_CURVE_WITH_KNOTS('',3,(#13172,#13173,#13174,#13175,#13176,
#13177,#13178,#13179,#13180,#13181,#13182,#13183),.UNSPECIFIED.,.F.,.F.,
(4,2,2,2,2,4),(0.0473477652366656,0.126350602536658,0.189525903804987,0.252701205073316,
0.313298422430275,0.373895639787233),.UNSPECIFIED.);
#456=B_SPLINE_CURVE_WITH_KNOTS('',3,(#13185,#13186,#13187,#13188,#13189,
#13190,#13191,#13192,#13193,#13194,#13195,#13196),.UNSPECIFIED.,.F.,.F.,
(4,2,2,2,2,4),(0.373895639787233,0.434492857144191,0.495090074501149,0.558265375769478,
0.621440677037807,0.7004435143378),.UNSPECIFIED.);
#457=B_SPLINE_CURVE_WITH_KNOTS('',3,(#13203,#13204,#13205,#13206,#13207,
#13208,#13209,#13210,#13211,#13212,#13213,#13214,#13215,#13216,#13217,#13218,
#13219,#13220,#13221,#13222,#13223,#13224),.UNSPECIFIED.,.F.,.F.,(4,2,2,
2,2,2,2,2,2,2,4),(0.0473477652366656,0.126350602536658,0.189525903804987,
0.252701205073316,0.313298422430275,0.373895639787233,0.434492857144191,
0.495090074501149,0.558265375769478,0.621440677037807,0.7004435143378),
 .UNSPECIFIED.);
#458=B_SPLINE_CURVE_WITH_KNOTS('',3,(#13232,#13233,#13234,#13235,#13236,
#13237,#13238,#13239,#13240,#13241,#13242,#13243,#13244,#13245,#13246,#13247,
#13248,#13249,#13250,#13251,#13252,#13253),.UNSPECIFIED.,.F.,.F.,(4,2,2,
2,2,2,2,2,2,2,4),(0.0473477652366656,0.126350602536658,0.189525903804987,
0.252701205073317,0.313298422430275,0.373895639787233,0.434492857144191,
0.495090074501149,0.558265375769478,0.621440677037807,0.7004435143378),
 .UNSPECIFIED.);
#459=B_SPLINE_CURVE_WITH_KNOTS('',3,(#13261,#13262,#13263,#13264,#13265,
#13266,#13267,#13268,#13269,#13270,#13271,#13272,#13273,#13274,#13275,#13276,
#13277,#13278,#13279,#13280,#13281,#13282),.UNSPECIFIED.,.F.,.F.,(4,2,2,
2,2,2,2,2,2,2,4),(0.0473477652366656,0.126350602536658,0.189525903804987,
0.252701205073316,0.313298422430275,0.373895639787233,0.434492857144191,
0.495090074501149,0.558265375769478,0.621440677037807,0.7004435143378),
 .UNSPECIFIED.);
#460=B_SPLINE_CURVE_WITH_KNOTS('',3,(#13291,#13292,#13293,#13294,#13295,
#13296,#13297,#13298,#13299,#13300,#13301,#13302,#13303,#13304,#13305,#13306,
#13307,#13308,#13309,#13310,#13311,#13312),.UNSPECIFIED.,.F.,.F.,(4,2,2,
2,2,2,2,2,2,2,4),(0.0473477652366656,0.126350602536658,0.189525903804987,
0.252701205073317,0.313298422430275,0.373895639787233,0.434492857144191,
0.495090074501149,0.558265375769478,0.621440677037807,0.7004435143378),
 .UNSPECIFIED.);
#461=SHAPE_REPRESENTATION_RELATIONSHIP('SRR','None',#13998,#495);
#462=SHAPE_REPRESENTATION_RELATIONSHIP('SRR','None',#13999,#496);
#463=SHAPE_REPRESENTATION_RELATIONSHIP('SRR','None',#14000,#497);
#464=SHAPE_REPRESENTATION_RELATIONSHIP('SRR','None',#14001,#498);
#465=SHAPE_REPRESENTATION_RELATIONSHIP('SRR','None',#14002,#499);
#466=SHAPE_REPRESENTATION_RELATIONSHIP('SRR','None',#14003,#500);
#467=SHAPE_REPRESENTATION_RELATIONSHIP('SRR','None',#14004,#501);
#468=SHAPE_REPRESENTATION_RELATIONSHIP('SRR','None',#14005,#502);
#469=SHAPE_REPRESENTATION_RELATIONSHIP('SRR','None',#14006,#503);
#470=SHAPE_REPRESENTATION_RELATIONSHIP('SRR','None',#14007,#504);
#471=SHAPE_REPRESENTATION_RELATIONSHIP('SRR','None',#14008,#505);
#472=SHAPE_REPRESENTATION_RELATIONSHIP('SRR','None',#14009,#506);
#473=SHAPE_REPRESENTATION_RELATIONSHIP('SRR','None',#14010,#507);
#474=SHAPE_REPRESENTATION_RELATIONSHIP('SRR','None',#14011,#508);
#475=SHAPE_REPRESENTATION_RELATIONSHIP('SRR','None',#14013,#509);
#476=SHAPE_REPRESENTATION_RELATIONSHIP('SRR','None',#14014,#510);
#477=SHAPE_REPRESENTATION_RELATIONSHIP('SRR','None',#14015,#511);
#478=SHAPE_REPRESENTATION_RELATIONSHIP('SRR','None',#14016,#512);
#479=SHAPE_REPRESENTATION_RELATIONSHIP('SRR','None',#14017,#513);
#480=SHAPE_REPRESENTATION_RELATIONSHIP('SRR','None',#14018,#514);
#481=SHAPE_REPRESENTATION_RELATIONSHIP('SRR','None',#14019,#515);
#482=SHAPE_REPRESENTATION_RELATIONSHIP('SRR','None',#14020,#516);
#483=SHAPE_REPRESENTATION_RELATIONSHIP('SRR','None',#14021,#517);
#484=SHAPE_REPRESENTATION_RELATIONSHIP('SRR','None',#14023,#518);
#485=SHAPE_REPRESENTATION_RELATIONSHIP('SRR','None',#14024,#519);
#486=SHAPE_REPRESENTATION_RELATIONSHIP('SRR','None',#14025,#520);
#487=SHAPE_REPRESENTATION_RELATIONSHIP('SRR','None',#14026,#521);
#488=SHAPE_REPRESENTATION_RELATIONSHIP('SRR','None',#14027,#522);
#489=SHAPE_REPRESENTATION_RELATIONSHIP('SRR','None',#14028,#523);
#490=SHAPE_REPRESENTATION_RELATIONSHIP('SRR','None',#14029,#524);
#491=SHAPE_REPRESENTATION_RELATIONSHIP('SRR','None',#14030,#525);
#492=SHAPE_REPRESENTATION_RELATIONSHIP('SRR','None',#14031,#526);
#493=SHAPE_REPRESENTATION_RELATIONSHIP('SRR','None',#14032,#527);
#494=SHAPE_REPRESENTATION_RELATIONSHIP('SRR','None',#14033,#528);
#495=ADVANCED_BREP_SHAPE_REPRESENTATION('',(#571),#13785);
#496=ADVANCED_BREP_SHAPE_REPRESENTATION('',(#572),#13786);
#497=ADVANCED_BREP_SHAPE_REPRESENTATION('',(#573),#13787);
#498=ADVANCED_BREP_SHAPE_REPRESENTATION('',(#574),#13788);
#499=ADVANCED_BREP_SHAPE_REPRESENTATION('',(#429),#13789);
#500=ADVANCED_BREP_SHAPE_REPRESENTATION('',(#430),#13790);
#501=ADVANCED_BREP_SHAPE_REPRESENTATION('',(#575),#13791);
#502=ADVANCED_BREP_SHAPE_REPRESENTATION('',(#576),#13792);
#503=ADVANCED_BREP_SHAPE_REPRESENTATION('',(#577),#13793);
#504=ADVANCED_BREP_SHAPE_REPRESENTATION('',(#578),#13794);
#505=ADVANCED_BREP_SHAPE_REPRESENTATION('',(#579),#13795);
#506=ADVANCED_BREP_SHAPE_REPRESENTATION('',(#580),#13796);
#507=ADVANCED_BREP_SHAPE_REPRESENTATION('',(#581),#13797);
#508=ADVANCED_BREP_SHAPE_REPRESENTATION('',(#582),#13798);
#509=ADVANCED_BREP_SHAPE_REPRESENTATION('',(#583),#13800);
#510=ADVANCED_BREP_SHAPE_REPRESENTATION('',(#584),#13801);
#511=ADVANCED_BREP_SHAPE_REPRESENTATION('',(#585),#13802);
#512=ADVANCED_BREP_SHAPE_REPRESENTATION('',(#586),#13803);
#513=ADVANCED_BREP_SHAPE_REPRESENTATION('',(#587),#13804);
#514=ADVANCED_BREP_SHAPE_REPRESENTATION('',(#588),#13805);
#515=ADVANCED_BREP_SHAPE_REPRESENTATION('',(#589),#13806);
#516=ADVANCED_BREP_SHAPE_REPRESENTATION('',(#590),#13807);
#517=ADVANCED_BREP_SHAPE_REPRESENTATION('',(#591),#13808);
#518=ADVANCED_BREP_SHAPE_REPRESENTATION('',(#592),#13810);
#519=ADVANCED_BREP_SHAPE_REPRESENTATION('',(#593),#13811);
#520=ADVANCED_BREP_SHAPE_REPRESENTATION('',(#594,#595,#596,#597,#598,#599,
#600,#601),#13812);
#521=ADVANCED_BREP_SHAPE_REPRESENTATION('',(#602),#13813);
#522=ADVANCED_BREP_SHAPE_REPRESENTATION('',(#603,#604),#13814);
#523=ADVANCED_BREP_SHAPE_REPRESENTATION('',(#605),#13815);
#524=ADVANCED_BREP_SHAPE_REPRESENTATION('',(#431),#13816);
#525=ADVANCED_BREP_SHAPE_REPRESENTATION('',(#606),#13817);
#526=ADVANCED_BREP_SHAPE_REPRESENTATION('',(#607),#13818);
#527=ADVANCED_BREP_SHAPE_REPRESENTATION('',(#432),#13819);
#528=ADVANCED_BREP_SHAPE_REPRESENTATION('',(#608),#13820);
#529=STYLED_ITEM('',(#14191),#571);
#530=STYLED_ITEM('',(#14191),#572);
#531=STYLED_ITEM('',(#14191),#573);
#532=STYLED_ITEM('',(#14192),#574);
#533=STYLED_ITEM('',(#14193),#429);
#534=STYLED_ITEM('',(#14193),#430);
#535=STYLED_ITEM('',(#14191),#575);
#536=STYLED_ITEM('',(#14191),#576);
#537=STYLED_ITEM('',(#14194),#577);
#538=STYLED_ITEM('',(#14193),#578);
#539=STYLED_ITEM('',(#14193),#579);
#540=STYLED_ITEM('',(#14194),#580);
#541=STYLED_ITEM('',(#14193),#581);
#542=STYLED_ITEM('',(#14193),#582);
#543=STYLED_ITEM('',(#14192),#583);
#544=STYLED_ITEM('',(#14191),#584);
#545=STYLED_ITEM('',(#14191),#585);
#546=STYLED_ITEM('',(#14191),#586);
#547=STYLED_ITEM('',(#14191),#587);
#548=STYLED_ITEM('',(#14192),#588);
#549=STYLED_ITEM('',(#14192),#589);
#550=STYLED_ITEM('',(#14192),#590);
#551=STYLED_ITEM('',(#14191),#591);
#552=STYLED_ITEM('',(#14191),#592);
#553=STYLED_ITEM('',(#14191),#593);
#554=STYLED_ITEM('',(#14191),#594);
#555=STYLED_ITEM('',(#14191),#595);
#556=STYLED_ITEM('',(#14191),#596);
#557=STYLED_ITEM('',(#14191),#597);
#558=STYLED_ITEM('',(#14191),#598);
#559=STYLED_ITEM('',(#14191),#599);
#560=STYLED_ITEM('',(#14191),#600);
#561=STYLED_ITEM('',(#14191),#601);
#562=STYLED_ITEM('',(#14190),#602);
#563=STYLED_ITEM('',(#14192),#603);
#564=STYLED_ITEM('',(#14192),#604);
#565=STYLED_ITEM('',(#14191),#605);
#566=STYLED_ITEM('',(#14193),#431);
#567=STYLED_ITEM('',(#14192),#606);
#568=STYLED_ITEM('',(#14192),#607);
#569=STYLED_ITEM('',(#14193),#432);
#570=STYLED_ITEM('',(#14192),#608);
#571=MANIFOLD_SOLID_BREP('Body1',#7627);
#572=MANIFOLD_SOLID_BREP('Body1',#7628);
#573=MANIFOLD_SOLID_BREP('Body1',#7629);
#574=MANIFOLD_SOLID_BREP('Body1',#7630);
#575=MANIFOLD_SOLID_BREP('Body1',#7635);
#576=MANIFOLD_SOLID_BREP('Body1',#7636);
#577=MANIFOLD_SOLID_BREP('Body1',#7637);
#578=MANIFOLD_SOLID_BREP('Body1',#7638);
#579=MANIFOLD_SOLID_BREP('Body1',#7639);
#580=MANIFOLD_SOLID_BREP('Body1',#7640);
#581=MANIFOLD_SOLID_BREP('Body1',#7641);
#582=MANIFOLD_SOLID_BREP('Body1',#7642);
#583=MANIFOLD_SOLID_BREP('Body1',#7643);
#584=MANIFOLD_SOLID_BREP('Body1',#7644);
#585=MANIFOLD_SOLID_BREP('Body1',#7645);
#586=MANIFOLD_SOLID_BREP('Body1',#7646);
#587=MANIFOLD_SOLID_BREP('Body1',#7647);
#588=MANIFOLD_SOLID_BREP('Body1',#7648);
#589=MANIFOLD_SOLID_BREP('Body1',#7649);
#590=MANIFOLD_SOLID_BREP('Body1',#7650);
#591=MANIFOLD_SOLID_BREP('Body1',#7651);
#592=MANIFOLD_SOLID_BREP('Body1',#7652);
#593=MANIFOLD_SOLID_BREP('Body1',#7653);
#594=MANIFOLD_SOLID_BREP('Body1',#7654);
#595=MANIFOLD_SOLID_BREP('Body2',#7655);
#596=MANIFOLD_SOLID_BREP('Body3',#7656);
#597=MANIFOLD_SOLID_BREP('Body4',#7657);
#598=MANIFOLD_SOLID_BREP('Body5',#7658);
#599=MANIFOLD_SOLID_BREP('Body6',#7659);
#600=MANIFOLD_SOLID_BREP('Body7',#7660);
#601=MANIFOLD_SOLID_BREP('Body8',#7661);
#602=MANIFOLD_SOLID_BREP('Continuous crown cage',#7662);
#603=MANIFOLD_SOLID_BREP('Body1',#7663);
#604=MANIFOLD_SOLID_BREP('Body2',#7664);
#605=MANIFOLD_SOLID_BREP('Body1',#7665);
#606=MANIFOLD_SOLID_BREP('Body1',#7668);
#607=MANIFOLD_SOLID_BREP('Body1',#7669);
#608=MANIFOLD_SOLID_BREP('Body1',#7672);
#609=FACE_BOUND('',#1431,.T.);
#610=FACE_BOUND('',#1432,.T.);
#611=FACE_BOUND('',#1433,.T.);
#612=FACE_BOUND('',#1434,.T.);
#613=FACE_BOUND('',#1437,.T.);
#614=FACE_BOUND('',#1438,.T.);
#615=FACE_BOUND('',#1439,.T.);
#616=FACE_BOUND('',#1440,.T.);
#617=FACE_BOUND('',#1445,.T.);
#618=FACE_BOUND('',#1461,.T.);
#619=FACE_BOUND('',#1480,.T.);
#620=FACE_BOUND('',#1495,.T.);
#621=FACE_BOUND('',#1497,.T.);
#622=FACE_BOUND('',#1499,.T.);
#623=FACE_BOUND('',#1515,.T.);
#624=FACE_BOUND('',#1534,.T.);
#625=FACE_BOUND('',#1549,.T.);
#626=FACE_BOUND('',#1551,.T.);
#627=FACE_BOUND('',#1598,.T.);
#628=FACE_BOUND('',#1600,.T.);
#629=FACE_BOUND('',#1610,.T.);
#630=FACE_BOUND('',#1618,.T.);
#631=FACE_BOUND('',#1626,.T.);
#632=FACE_BOUND('',#1644,.T.);
#633=FACE_BOUND('',#1645,.T.);
#634=FACE_BOUND('',#1646,.T.);
#635=FACE_BOUND('',#1647,.T.);
#636=FACE_BOUND('',#1650,.T.);
#637=FACE_BOUND('',#1651,.T.);
#638=FACE_BOUND('',#1652,.T.);
#639=FACE_BOUND('',#1653,.T.);
#640=FACE_BOUND('',#1660,.T.);
#641=FACE_BOUND('',#1663,.T.);
#642=FACE_BOUND('',#1671,.T.);
#643=FACE_BOUND('',#1672,.T.);
#644=FACE_BOUND('',#1674,.T.);
#645=FACE_BOUND('',#1675,.T.);
#646=FACE_BOUND('',#1695,.T.);
#647=FACE_BOUND('',#1696,.T.);
#648=FACE_BOUND('',#1698,.T.);
#649=FACE_BOUND('',#1699,.T.);
#650=FACE_BOUND('',#1715,.T.);
#651=FACE_BOUND('',#1717,.T.);
#652=FACE_BOUND('',#1720,.T.);
#653=FACE_BOUND('',#1724,.T.);
#654=FACE_BOUND('',#1726,.T.);
#655=FACE_BOUND('',#1729,.T.);
#656=FACE_BOUND('',#1733,.T.);
#657=FACE_BOUND('',#1735,.T.);
#658=FACE_BOUND('',#1738,.T.);
#659=FACE_BOUND('',#1742,.T.);
#660=FACE_BOUND('',#1744,.T.);
#661=FACE_BOUND('',#1747,.T.);
#662=FACE_BOUND('',#1751,.T.);
#663=FACE_BOUND('',#1753,.T.);
#664=FACE_BOUND('',#1760,.T.);
#665=FACE_BOUND('',#1762,.T.);
#666=FACE_BOUND('',#1765,.T.);
#667=FACE_BOUND('',#1768,.T.);
#668=FACE_BOUND('',#1773,.T.);
#669=FACE_BOUND('',#1776,.T.);
#670=FACE_BOUND('',#1779,.T.);
#671=FACE_BOUND('',#1780,.T.);
#672=FACE_BOUND('',#1782,.T.);
#673=FACE_BOUND('',#1783,.T.);
#674=FACE_BOUND('',#1787,.T.);
#675=FACE_BOUND('',#1789,.T.);
#676=FACE_BOUND('',#1793,.T.);
#677=FACE_BOUND('',#1795,.T.);
#678=FACE_BOUND('',#1801,.T.);
#679=FACE_BOUND('',#1804,.T.);
#680=FACE_BOUND('',#1809,.T.);
#681=FACE_BOUND('',#1814,.T.);
#682=FACE_BOUND('',#1842,.T.);
#683=FACE_BOUND('',#1845,.T.);
#684=FACE_BOUND('',#1848,.T.);
#685=FACE_BOUND('',#1851,.T.);
#686=FACE_BOUND('',#1854,.T.);
#687=FACE_BOUND('',#1859,.T.);
#688=FACE_BOUND('',#1861,.T.);
#689=FACE_BOUND('',#1876,.T.);
#690=FACE_BOUND('',#1882,.T.);
#691=FACE_BOUND('',#1884,.T.);
#692=FACE_BOUND('',#1888,.T.);
#693=FACE_BOUND('',#1914,.T.);
#694=FACE_BOUND('',#1919,.T.);
#695=FACE_BOUND('',#1922,.T.);
#696=FACE_BOUND('',#1927,.T.);
#697=FACE_BOUND('',#1930,.T.);
#698=FACE_BOUND('',#1933,.T.);
#699=FACE_BOUND('',#1934,.T.);
#700=FACE_BOUND('',#1936,.T.);
#701=FACE_BOUND('',#1937,.T.);
#702=PLANE('',#8063);
#703=PLANE('',#8064);
#704=PLANE('',#8065);
#705=PLANE('',#8066);
#706=PLANE('',#8067);
#707=PLANE('',#8068);
#708=PLANE('',#8075);
#709=PLANE('',#8076);
#710=PLANE('',#8077);
#711=PLANE('',#8078);
#712=PLANE('',#8079);
#713=PLANE('',#8080);
#714=PLANE('',#8081);
#715=PLANE('',#8082);
#716=PLANE('',#8083);
#717=PLANE('',#8084);
#718=PLANE('',#8085);
#719=PLANE('',#8086);
#720=PLANE('',#8087);
#721=PLANE('',#8088);
#722=PLANE('',#8089);
#723=PLANE('',#8090);
#724=PLANE('',#8091);
#725=PLANE('',#8092);
#726=PLANE('',#8093);
#727=PLANE('',#8094);
#728=PLANE('',#8095);
#729=PLANE('',#8096);
#730=PLANE('',#8097);
#731=PLANE('',#8098);
#732=PLANE('',#8099);
#733=PLANE('',#8100);
#734=PLANE('',#8101);
#735=PLANE('',#8102);
#736=PLANE('',#8103);
#737=PLANE('',#8104);
#738=PLANE('',#8105);
#739=PLANE('',#8106);
#740=PLANE('',#8107);
#741=PLANE('',#8108);
#742=PLANE('',#8109);
#743=PLANE('',#8110);
#744=PLANE('',#8113);
#745=PLANE('',#8114);
#746=PLANE('',#8115);
#747=PLANE('',#8116);
#748=PLANE('',#8117);
#749=PLANE('',#8118);
#750=PLANE('',#8119);
#751=PLANE('',#8120);
#752=PLANE('',#8121);
#753=PLANE('',#8122);
#754=PLANE('',#8129);
#755=PLANE('',#8130);
#756=PLANE('',#8131);
#757=PLANE('',#8132);
#758=PLANE('',#8133);
#759=PLANE('',#8134);
#760=PLANE('',#8135);
#761=PLANE('',#8136);
#762=PLANE('',#8137);
#763=PLANE('',#8138);
#764=PLANE('',#8139);
#765=PLANE('',#8140);
#766=PLANE('',#8141);
#767=PLANE('',#8142);
#768=PLANE('',#8143);
#769=PLANE('',#8144);
#770=PLANE('',#8145);
#771=PLANE('',#8146);
#772=PLANE('',#8147);
#773=PLANE('',#8148);
#774=PLANE('',#8149);
#775=PLANE('',#8150);
#776=PLANE('',#8151);
#777=PLANE('',#8152);
#778=PLANE('',#8153);
#779=PLANE('',#8154);
#780=PLANE('',#8155);
#781=PLANE('',#8156);
#782=PLANE('',#8157);
#783=PLANE('',#8158);
#784=PLANE('',#8159);
#785=PLANE('',#8160);
#786=PLANE('',#8161);
#787=PLANE('',#8162);
#788=PLANE('',#8163);
#789=PLANE('',#8164);
#790=PLANE('',#8167);
#791=PLANE('',#8168);
#792=PLANE('',#8169);
#793=PLANE('',#8170);
#794=PLANE('',#8171);
#795=PLANE('',#8172);
#796=PLANE('',#8173);
#797=PLANE('',#8174);
#798=PLANE('',#8175);
#799=PLANE('',#8176);
#800=PLANE('',#8178);
#801=PLANE('',#8179);
#802=PLANE('',#8180);
#803=PLANE('',#8181);
#804=PLANE('',#8182);
#805=PLANE('',#8183);
#806=PLANE('',#8184);
#807=PLANE('',#8185);
#808=PLANE('',#8186);
#809=PLANE('',#8187);
#810=PLANE('',#8188);
#811=PLANE('',#8189);
#812=PLANE('',#8190);
#813=PLANE('',#8191);
#814=PLANE('',#8192);
#815=PLANE('',#8193);
#816=PLANE('',#8194);
#817=PLANE('',#8195);
#818=PLANE('',#8196);
#819=PLANE('',#8197);
#820=PLANE('',#8198);
#821=PLANE('',#8199);
#822=PLANE('',#8200);
#823=PLANE('',#8201);
#824=PLANE('',#8202);
#825=PLANE('',#8203);
#826=PLANE('',#8204);
#827=PLANE('',#8205);
#828=PLANE('',#8206);
#829=PLANE('',#8207);
#830=PLANE('',#8208);
#831=PLANE('',#8209);
#832=PLANE('',#8210);
#833=PLANE('',#8211);
#834=PLANE('',#8212);
#835=PLANE('',#8213);
#836=PLANE('',#8217);
#837=PLANE('',#8218);
#838=PLANE('',#8219);
#839=PLANE('',#8220);
#840=PLANE('',#8221);
#841=PLANE('',#8222);
#842=PLANE('',#8223);
#843=PLANE('',#8224);
#844=PLANE('',#8225);
#845=PLANE('',#8226);
#846=PLANE('',#8228);
#847=PLANE('',#8229);
#848=PLANE('',#8230);
#849=PLANE('',#8231);
#850=PLANE('',#8232);
#851=PLANE('',#8233);
#852=PLANE('',#8234);
#853=PLANE('',#8235);
#854=PLANE('',#8236);
#855=PLANE('',#8241);
#856=PLANE('',#8242);
#857=PLANE('',#8250);
#858=PLANE('',#8256);
#859=PLANE('',#8264);
#860=PLANE('',#8272);
#861=PLANE('',#8273);
#862=PLANE('',#8274);
#863=PLANE('',#8275);
#864=PLANE('',#8276);
#865=PLANE('',#8277);
#866=PLANE('',#8278);
#867=PLANE('',#8279);
#868=PLANE('',#8280);
#869=PLANE('',#8294);
#870=PLANE('',#8295);
#871=PLANE('',#8296);
#872=PLANE('',#8297);
#873=PLANE('',#8298);
#874=PLANE('',#8299);
#875=PLANE('',#8306);
#876=PLANE('',#8310);
#877=PLANE('',#8318);
#878=PLANE('',#8319);
#879=PLANE('',#8320);
#880=PLANE('',#8321);
#881=PLANE('',#8322);
#882=PLANE('',#8323);
#883=PLANE('',#8325);
#884=PLANE('',#8326);
#885=PLANE('',#8327);
#886=PLANE('',#8328);
#887=PLANE('',#8329);
#888=PLANE('',#8330);
#889=PLANE('',#8332);
#890=PLANE('',#8333);
#891=PLANE('',#8334);
#892=PLANE('',#8335);
#893=PLANE('',#8336);
#894=PLANE('',#8337);
#895=PLANE('',#8345);
#896=PLANE('',#8346);
#897=PLANE('',#8347);
#898=PLANE('',#8348);
#899=PLANE('',#8349);
#900=PLANE('',#8350);
#901=PLANE('',#8352);
#902=PLANE('',#8353);
#903=PLANE('',#8354);
#904=PLANE('',#8355);
#905=PLANE('',#8356);
#906=PLANE('',#8357);
#907=PLANE('',#8359);
#908=PLANE('',#8360);
#909=PLANE('',#8361);
#910=PLANE('',#8362);
#911=PLANE('',#8363);
#912=PLANE('',#8364);
#913=PLANE('',#8373);
#914=PLANE('',#8374);
#915=PLANE('',#8379);
#916=PLANE('',#8386);
#917=PLANE('',#8387);
#918=PLANE('',#8392);
#919=PLANE('',#8399);
#920=PLANE('',#8400);
#921=PLANE('',#8405);
#922=PLANE('',#8412);
#923=PLANE('',#8413);
#924=PLANE('',#8418);
#925=PLANE('',#8425);
#926=PLANE('',#8426);
#927=PLANE('',#8431);
#928=PLANE('',#8435);
#929=PLANE('',#8439);
#930=PLANE('',#8440);
#931=PLANE('',#8445);
#932=PLANE('',#8450);
#933=PLANE('',#8459);
#934=PLANE('',#8460);
#935=PLANE('',#8461);
#936=PLANE('',#8462);
#937=PLANE('',#8463);
#938=PLANE('',#8464);
#939=PLANE('',#8472);
#940=PLANE('',#8473);
#941=PLANE('',#8481);
#942=PLANE('',#8482);
#943=PLANE('',#8498);
#944=PLANE('',#8501);
#945=PLANE('',#8513);
#946=PLANE('',#8522);
#947=PLANE('',#8555);
#948=PLANE('',#8560);
#949=PLANE('',#8565);
#950=PLANE('',#8570);
#951=PLANE('',#8575);
#952=PLANE('',#8580);
#953=PLANE('',#8589);
#954=PLANE('',#8593);
#955=PLANE('',#8594);
#956=PLANE('',#8596);
#957=PLANE('',#8601);
#958=PLANE('',#8604);
#959=PLANE('',#8609);
#960=PLANE('',#8624);
#961=PLANE('',#8625);
#962=PLANE('',#8627);
#963=PLANE('',#8628);
#964=PLANE('',#8629);
#965=PLANE('',#8630);
#966=PLANE('',#8631);
#967=PLANE('',#8632);
#968=PLANE('',#8633);
#969=PLANE('',#8634);
#970=PLANE('',#8635);
#971=PLANE('',#8637);
#972=PLANE('',#8645);
#973=PLANE('',#8657);
#974=PLANE('',#8658);
#975=PLANE('',#8660);
#976=PLANE('',#8661);
#977=PLANE('',#8662);
#978=PLANE('',#8664);
#979=PLANE('',#8665);
#980=PLANE('',#8666);
#981=PLANE('',#8667);
#982=PLANE('',#8668);
#983=PLANE('',#8669);
#984=PLANE('',#8676);
#985=PLANE('',#8677);
#986=PLANE('',#8678);
#987=PLANE('',#8679);
#988=PLANE('',#8681);
#989=PLANE('',#8682);
#990=PLANE('',#8683);
#991=PLANE('',#8684);
#992=PLANE('',#8685);
#993=PLANE('',#8686);
#994=PLANE('',#8687);
#995=PLANE('',#8688);
#996=PLANE('',#8689);
#997=PLANE('',#8691);
#998=PLANE('',#8699);
#999=PLANE('',#8764);
#1000=PLANE('',#8769);
#1001=PLANE('',#8778);
#1002=PLANE('',#8779);
#1003=PLANE('',#8780);
#1004=PLANE('',#8781);
#1005=PLANE('',#8782);
#1006=PLANE('',#8783);
#1007=FACE_OUTER_BOUND('',#1426,.T.);
#1008=FACE_OUTER_BOUND('',#1427,.T.);
#1009=FACE_OUTER_BOUND('',#1428,.T.);
#1010=FACE_OUTER_BOUND('',#1429,.T.);
#1011=FACE_OUTER_BOUND('',#1430,.T.);
#1012=FACE_OUTER_BOUND('',#1435,.T.);
#1013=FACE_OUTER_BOUND('',#1436,.T.);
#1014=FACE_OUTER_BOUND('',#1441,.T.);
#1015=FACE_OUTER_BOUND('',#1442,.T.);
#1016=FACE_OUTER_BOUND('',#1443,.T.);
#1017=FACE_OUTER_BOUND('',#1444,.T.);
#1018=FACE_OUTER_BOUND('',#1446,.T.);
#1019=FACE_OUTER_BOUND('',#1447,.T.);
#1020=FACE_OUTER_BOUND('',#1448,.T.);
#1021=FACE_OUTER_BOUND('',#1449,.T.);
#1022=FACE_OUTER_BOUND('',#1450,.T.);
#1023=FACE_OUTER_BOUND('',#1451,.T.);
#1024=FACE_OUTER_BOUND('',#1452,.T.);
#1025=FACE_OUTER_BOUND('',#1453,.T.);
#1026=FACE_OUTER_BOUND('',#1454,.T.);
#1027=FACE_OUTER_BOUND('',#1455,.T.);
#1028=FACE_OUTER_BOUND('',#1456,.T.);
#1029=FACE_OUTER_BOUND('',#1457,.T.);
#1030=FACE_OUTER_BOUND('',#1458,.T.);
#1031=FACE_OUTER_BOUND('',#1459,.T.);
#1032=FACE_OUTER_BOUND('',#1460,.T.);
#1033=FACE_OUTER_BOUND('',#1462,.T.);
#1034=FACE_OUTER_BOUND('',#1463,.T.);
#1035=FACE_OUTER_BOUND('',#1464,.T.);
#1036=FACE_OUTER_BOUND('',#1465,.T.);
#1037=FACE_OUTER_BOUND('',#1466,.T.);
#1038=FACE_OUTER_BOUND('',#1467,.T.);
#1039=FACE_OUTER_BOUND('',#1468,.T.);
#1040=FACE_OUTER_BOUND('',#1469,.T.);
#1041=FACE_OUTER_BOUND('',#1470,.T.);
#1042=FACE_OUTER_BOUND('',#1471,.T.);
#1043=FACE_OUTER_BOUND('',#1472,.T.);
#1044=FACE_OUTER_BOUND('',#1473,.T.);
#1045=FACE_OUTER_BOUND('',#1474,.T.);
#1046=FACE_OUTER_BOUND('',#1475,.T.);
#1047=FACE_OUTER_BOUND('',#1476,.T.);
#1048=FACE_OUTER_BOUND('',#1477,.T.);
#1049=FACE_OUTER_BOUND('',#1478,.T.);
#1050=FACE_OUTER_BOUND('',#1479,.T.);
#1051=FACE_OUTER_BOUND('',#1481,.T.);
#1052=FACE_OUTER_BOUND('',#1482,.T.);
#1053=FACE_OUTER_BOUND('',#1483,.T.);
#1054=FACE_OUTER_BOUND('',#1484,.T.);
#1055=FACE_OUTER_BOUND('',#1485,.T.);
#1056=FACE_OUTER_BOUND('',#1486,.T.);
#1057=FACE_OUTER_BOUND('',#1487,.T.);
#1058=FACE_OUTER_BOUND('',#1488,.T.);
#1059=FACE_OUTER_BOUND('',#1489,.T.);
#1060=FACE_OUTER_BOUND('',#1490,.T.);
#1061=FACE_OUTER_BOUND('',#1491,.T.);
#1062=FACE_OUTER_BOUND('',#1492,.T.);
#1063=FACE_OUTER_BOUND('',#1493,.T.);
#1064=FACE_OUTER_BOUND('',#1494,.T.);
#1065=FACE_OUTER_BOUND('',#1496,.T.);
#1066=FACE_OUTER_BOUND('',#1498,.T.);
#1067=FACE_OUTER_BOUND('',#1500,.T.);
#1068=FACE_OUTER_BOUND('',#1501,.T.);
#1069=FACE_OUTER_BOUND('',#1502,.T.);
#1070=FACE_OUTER_BOUND('',#1503,.T.);
#1071=FACE_OUTER_BOUND('',#1504,.T.);
#1072=FACE_OUTER_BOUND('',#1505,.T.);
#1073=FACE_OUTER_BOUND('',#1506,.T.);
#1074=FACE_OUTER_BOUND('',#1507,.T.);
#1075=FACE_OUTER_BOUND('',#1508,.T.);
#1076=FACE_OUTER_BOUND('',#1509,.T.);
#1077=FACE_OUTER_BOUND('',#1510,.T.);
#1078=FACE_OUTER_BOUND('',#1511,.T.);
#1079=FACE_OUTER_BOUND('',#1512,.T.);
#1080=FACE_OUTER_BOUND('',#1513,.T.);
#1081=FACE_OUTER_BOUND('',#1514,.T.);
#1082=FACE_OUTER_BOUND('',#1516,.T.);
#1083=FACE_OUTER_BOUND('',#1517,.T.);
#1084=FACE_OUTER_BOUND('',#1518,.T.);
#1085=FACE_OUTER_BOUND('',#1519,.T.);
#1086=FACE_OUTER_BOUND('',#1520,.T.);
#1087=FACE_OUTER_BOUND('',#1521,.T.);
#1088=FACE_OUTER_BOUND('',#1522,.T.);
#1089=FACE_OUTER_BOUND('',#1523,.T.);
#1090=FACE_OUTER_BOUND('',#1524,.T.);
#1091=FACE_OUTER_BOUND('',#1525,.T.);
#1092=FACE_OUTER_BOUND('',#1526,.T.);
#1093=FACE_OUTER_BOUND('',#1527,.T.);
#1094=FACE_OUTER_BOUND('',#1528,.T.);
#1095=FACE_OUTER_BOUND('',#1529,.T.);
#1096=FACE_OUTER_BOUND('',#1530,.T.);
#1097=FACE_OUTER_BOUND('',#1531,.T.);
#1098=FACE_OUTER_BOUND('',#1532,.T.);
#1099=FACE_OUTER_BOUND('',#1533,.T.);
#1100=FACE_OUTER_BOUND('',#1535,.T.);
#1101=FACE_OUTER_BOUND('',#1536,.T.);
#1102=FACE_OUTER_BOUND('',#1537,.T.);
#1103=FACE_OUTER_BOUND('',#1538,.T.);
#1104=FACE_OUTER_BOUND('',#1539,.T.);
#1105=FACE_OUTER_BOUND('',#1540,.T.);
#1106=FACE_OUTER_BOUND('',#1541,.T.);
#1107=FACE_OUTER_BOUND('',#1542,.T.);
#1108=FACE_OUTER_BOUND('',#1543,.T.);
#1109=FACE_OUTER_BOUND('',#1544,.T.);
#1110=FACE_OUTER_BOUND('',#1545,.T.);
#1111=FACE_OUTER_BOUND('',#1546,.T.);
#1112=FACE_OUTER_BOUND('',#1547,.T.);
#1113=FACE_OUTER_BOUND('',#1548,.T.);
#1114=FACE_OUTER_BOUND('',#1550,.T.);
#1115=FACE_OUTER_BOUND('',#1552,.T.);
#1116=FACE_OUTER_BOUND('',#1553,.T.);
#1117=FACE_OUTER_BOUND('',#1554,.T.);
#1118=FACE_OUTER_BOUND('',#1555,.T.);
#1119=FACE_OUTER_BOUND('',#1556,.T.);
#1120=FACE_OUTER_BOUND('',#1557,.T.);
#1121=FACE_OUTER_BOUND('',#1558,.T.);
#1122=FACE_OUTER_BOUND('',#1559,.T.);
#1123=FACE_OUTER_BOUND('',#1560,.T.);
#1124=FACE_OUTER_BOUND('',#1561,.T.);
#1125=FACE_OUTER_BOUND('',#1562,.T.);
#1126=FACE_OUTER_BOUND('',#1563,.T.);
#1127=FACE_OUTER_BOUND('',#1564,.T.);
#1128=FACE_OUTER_BOUND('',#1565,.T.);
#1129=FACE_OUTER_BOUND('',#1566,.T.);
#1130=FACE_OUTER_BOUND('',#1567,.T.);
#1131=FACE_OUTER_BOUND('',#1568,.T.);
#1132=FACE_OUTER_BOUND('',#1569,.T.);
#1133=FACE_OUTER_BOUND('',#1570,.T.);
#1134=FACE_OUTER_BOUND('',#1571,.T.);
#1135=FACE_OUTER_BOUND('',#1572,.T.);
#1136=FACE_OUTER_BOUND('',#1573,.T.);
#1137=FACE_OUTER_BOUND('',#1574,.T.);
#1138=FACE_OUTER_BOUND('',#1575,.T.);
#1139=FACE_OUTER_BOUND('',#1576,.T.);
#1140=FACE_OUTER_BOUND('',#1577,.T.);
#1141=FACE_OUTER_BOUND('',#1578,.T.);
#1142=FACE_OUTER_BOUND('',#1579,.T.);
#1143=FACE_OUTER_BOUND('',#1580,.T.);
#1144=FACE_OUTER_BOUND('',#1581,.T.);
#1145=FACE_OUTER_BOUND('',#1582,.T.);
#1146=FACE_OUTER_BOUND('',#1583,.T.);
#1147=FACE_OUTER_BOUND('',#1584,.T.);
#1148=FACE_OUTER_BOUND('',#1585,.T.);
#1149=FACE_OUTER_BOUND('',#1586,.T.);
#1150=FACE_OUTER_BOUND('',#1587,.T.);
#1151=FACE_OUTER_BOUND('',#1588,.T.);
#1152=FACE_OUTER_BOUND('',#1589,.T.);
#1153=FACE_OUTER_BOUND('',#1590,.T.);
#1154=FACE_OUTER_BOUND('',#1591,.T.);
#1155=FACE_OUTER_BOUND('',#1592,.T.);
#1156=FACE_OUTER_BOUND('',#1593,.T.);
#1157=FACE_OUTER_BOUND('',#1594,.T.);
#1158=FACE_OUTER_BOUND('',#1595,.T.);
#1159=FACE_OUTER_BOUND('',#1596,.T.);
#1160=FACE_OUTER_BOUND('',#1597,.T.);
#1161=FACE_OUTER_BOUND('',#1599,.T.);
#1162=FACE_OUTER_BOUND('',#1601,.T.);
#1163=FACE_OUTER_BOUND('',#1602,.T.);
#1164=FACE_OUTER_BOUND('',#1603,.T.);
#1165=FACE_OUTER_BOUND('',#1604,.T.);
#1166=FACE_OUTER_BOUND('',#1605,.T.);
#1167=FACE_OUTER_BOUND('',#1606,.T.);
#1168=FACE_OUTER_BOUND('',#1607,.T.);
#1169=FACE_OUTER_BOUND('',#1608,.T.);
#1170=FACE_OUTER_BOUND('',#1609,.T.);
#1171=FACE_OUTER_BOUND('',#1611,.T.);
#1172=FACE_OUTER_BOUND('',#1612,.T.);
#1173=FACE_OUTER_BOUND('',#1613,.T.);
#1174=FACE_OUTER_BOUND('',#1614,.T.);
#1175=FACE_OUTER_BOUND('',#1615,.T.);
#1176=FACE_OUTER_BOUND('',#1616,.T.);
#1177=FACE_OUTER_BOUND('',#1617,.T.);
#1178=FACE_OUTER_BOUND('',#1619,.T.);
#1179=FACE_OUTER_BOUND('',#1620,.T.);
#1180=FACE_OUTER_BOUND('',#1621,.T.);
#1181=FACE_OUTER_BOUND('',#1622,.T.);
#1182=FACE_OUTER_BOUND('',#1623,.T.);
#1183=FACE_OUTER_BOUND('',#1624,.T.);
#1184=FACE_OUTER_BOUND('',#1625,.T.);
#1185=FACE_OUTER_BOUND('',#1627,.T.);
#1186=FACE_OUTER_BOUND('',#1628,.T.);
#1187=FACE_OUTER_BOUND('',#1629,.T.);
#1188=FACE_OUTER_BOUND('',#1630,.T.);
#1189=FACE_OUTER_BOUND('',#1631,.T.);
#1190=FACE_OUTER_BOUND('',#1632,.T.);
#1191=FACE_OUTER_BOUND('',#1633,.T.);
#1192=FACE_OUTER_BOUND('',#1634,.T.);
#1193=FACE_OUTER_BOUND('',#1635,.T.);
#1194=FACE_OUTER_BOUND('',#1636,.T.);
#1195=FACE_OUTER_BOUND('',#1637,.T.);
#1196=FACE_OUTER_BOUND('',#1638,.T.);
#1197=FACE_OUTER_BOUND('',#1639,.T.);
#1198=FACE_OUTER_BOUND('',#1640,.T.);
#1199=FACE_OUTER_BOUND('',#1641,.T.);
#1200=FACE_OUTER_BOUND('',#1642,.T.);
#1201=FACE_OUTER_BOUND('',#1643,.T.);
#1202=FACE_OUTER_BOUND('',#1648,.T.);
#1203=FACE_OUTER_BOUND('',#1649,.T.);
#1204=FACE_OUTER_BOUND('',#1654,.T.);
#1205=FACE_OUTER_BOUND('',#1655,.T.);
#1206=FACE_OUTER_BOUND('',#1656,.T.);
#1207=FACE_OUTER_BOUND('',#1657,.T.);
#1208=FACE_OUTER_BOUND('',#1658,.T.);
#1209=FACE_OUTER_BOUND('',#1659,.T.);
#1210=FACE_OUTER_BOUND('',#1661,.T.);
#1211=FACE_OUTER_BOUND('',#1662,.T.);
#1212=FACE_OUTER_BOUND('',#1664,.T.);
#1213=FACE_OUTER_BOUND('',#1665,.T.);
#1214=FACE_OUTER_BOUND('',#1666,.T.);
#1215=FACE_OUTER_BOUND('',#1667,.T.);
#1216=FACE_OUTER_BOUND('',#1668,.T.);
#1217=FACE_OUTER_BOUND('',#1669,.T.);
#1218=FACE_OUTER_BOUND('',#1670,.T.);
#1219=FACE_OUTER_BOUND('',#1673,.T.);
#1220=FACE_OUTER_BOUND('',#1676,.T.);
#1221=FACE_OUTER_BOUND('',#1677,.T.);
#1222=FACE_OUTER_BOUND('',#1678,.T.);
#1223=FACE_OUTER_BOUND('',#1679,.T.);
#1224=FACE_OUTER_BOUND('',#1680,.T.);
#1225=FACE_OUTER_BOUND('',#1681,.T.);
#1226=FACE_OUTER_BOUND('',#1682,.T.);
#1227=FACE_OUTER_BOUND('',#1683,.T.);
#1228=FACE_OUTER_BOUND('',#1684,.T.);
#1229=FACE_OUTER_BOUND('',#1685,.T.);
#1230=FACE_OUTER_BOUND('',#1686,.T.);
#1231=FACE_OUTER_BOUND('',#1687,.T.);
#1232=FACE_OUTER_BOUND('',#1688,.T.);
#1233=FACE_OUTER_BOUND('',#1689,.T.);
#1234=FACE_OUTER_BOUND('',#1690,.T.);
#1235=FACE_OUTER_BOUND('',#1691,.T.);
#1236=FACE_OUTER_BOUND('',#1692,.T.);
#1237=FACE_OUTER_BOUND('',#1693,.T.);
#1238=FACE_OUTER_BOUND('',#1694,.T.);
#1239=FACE_OUTER_BOUND('',#1697,.T.);
#1240=FACE_OUTER_BOUND('',#1700,.T.);
#1241=FACE_OUTER_BOUND('',#1701,.T.);
#1242=FACE_OUTER_BOUND('',#1702,.T.);
#1243=FACE_OUTER_BOUND('',#1703,.T.);
#1244=FACE_OUTER_BOUND('',#1704,.T.);
#1245=FACE_OUTER_BOUND('',#1705,.T.);
#1246=FACE_OUTER_BOUND('',#1706,.T.);
#1247=FACE_OUTER_BOUND('',#1707,.T.);
#1248=FACE_OUTER_BOUND('',#1708,.T.);
#1249=FACE_OUTER_BOUND('',#1709,.T.);
#1250=FACE_OUTER_BOUND('',#1710,.T.);
#1251=FACE_OUTER_BOUND('',#1711,.T.);
#1252=FACE_OUTER_BOUND('',#1712,.T.);
#1253=FACE_OUTER_BOUND('',#1713,.T.);
#1254=FACE_OUTER_BOUND('',#1714,.T.);
#1255=FACE_OUTER_BOUND('',#1716,.T.);
#1256=FACE_OUTER_BOUND('',#1718,.T.);
#1257=FACE_OUTER_BOUND('',#1719,.T.);
#1258=FACE_OUTER_BOUND('',#1721,.T.);
#1259=FACE_OUTER_BOUND('',#1722,.T.);
#1260=FACE_OUTER_BOUND('',#1723,.T.);
#1261=FACE_OUTER_BOUND('',#1725,.T.);
#1262=FACE_OUTER_BOUND('',#1727,.T.);
#1263=FACE_OUTER_BOUND('',#1728,.T.);
#1264=FACE_OUTER_BOUND('',#1730,.T.);
#1265=FACE_OUTER_BOUND('',#1731,.T.);
#1266=FACE_OUTER_BOUND('',#1732,.T.);
#1267=FACE_OUTER_BOUND('',#1734,.T.);
#1268=FACE_OUTER_BOUND('',#1736,.T.);
#1269=FACE_OUTER_BOUND('',#1737,.T.);
#1270=FACE_OUTER_BOUND('',#1739,.T.);
#1271=FACE_OUTER_BOUND('',#1740,.T.);
#1272=FACE_OUTER_BOUND('',#1741,.T.);
#1273=FACE_OUTER_BOUND('',#1743,.T.);
#1274=FACE_OUTER_BOUND('',#1745,.T.);
#1275=FACE_OUTER_BOUND('',#1746,.T.);
#1276=FACE_OUTER_BOUND('',#1748,.T.);
#1277=FACE_OUTER_BOUND('',#1749,.T.);
#1278=FACE_OUTER_BOUND('',#1750,.T.);
#1279=FACE_OUTER_BOUND('',#1752,.T.);
#1280=FACE_OUTER_BOUND('',#1754,.T.);
#1281=FACE_OUTER_BOUND('',#1755,.T.);
#1282=FACE_OUTER_BOUND('',#1756,.T.);
#1283=FACE_OUTER_BOUND('',#1757,.T.);
#1284=FACE_OUTER_BOUND('',#1758,.T.);
#1285=FACE_OUTER_BOUND('',#1759,.T.);
#1286=FACE_OUTER_BOUND('',#1761,.T.);
#1287=FACE_OUTER_BOUND('',#1763,.T.);
#1288=FACE_OUTER_BOUND('',#1764,.T.);
#1289=FACE_OUTER_BOUND('',#1766,.T.);
#1290=FACE_OUTER_BOUND('',#1767,.T.);
#1291=FACE_OUTER_BOUND('',#1769,.T.);
#1292=FACE_OUTER_BOUND('',#1770,.T.);
#1293=FACE_OUTER_BOUND('',#1771,.T.);
#1294=FACE_OUTER_BOUND('',#1772,.T.);
#1295=FACE_OUTER_BOUND('',#1774,.T.);
#1296=FACE_OUTER_BOUND('',#1775,.T.);
#1297=FACE_OUTER_BOUND('',#1777,.T.);
#1298=FACE_OUTER_BOUND('',#1778,.T.);
#1299=FACE_OUTER_BOUND('',#1781,.T.);
#1300=FACE_OUTER_BOUND('',#1784,.T.);
#1301=FACE_OUTER_BOUND('',#1785,.T.);
#1302=FACE_OUTER_BOUND('',#1786,.T.);
#1303=FACE_OUTER_BOUND('',#1788,.T.);
#1304=FACE_OUTER_BOUND('',#1790,.T.);
#1305=FACE_OUTER_BOUND('',#1791,.T.);
#1306=FACE_OUTER_BOUND('',#1792,.T.);
#1307=FACE_OUTER_BOUND('',#1794,.T.);
#1308=FACE_OUTER_BOUND('',#1796,.T.);
#1309=FACE_OUTER_BOUND('',#1797,.T.);
#1310=FACE_OUTER_BOUND('',#1798,.T.);
#1311=FACE_OUTER_BOUND('',#1799,.T.);
#1312=FACE_OUTER_BOUND('',#1800,.T.);
#1313=FACE_OUTER_BOUND('',#1802,.T.);
#1314=FACE_OUTER_BOUND('',#1803,.T.);
#1315=FACE_OUTER_BOUND('',#1805,.T.);
#1316=FACE_OUTER_BOUND('',#1806,.T.);
#1317=FACE_OUTER_BOUND('',#1807,.T.);
#1318=FACE_OUTER_BOUND('',#1808,.T.);
#1319=FACE_OUTER_BOUND('',#1810,.T.);
#1320=FACE_OUTER_BOUND('',#1811,.T.);
#1321=FACE_OUTER_BOUND('',#1812,.T.);
#1322=FACE_OUTER_BOUND('',#1813,.T.);
#1323=FACE_OUTER_BOUND('',#1815,.T.);
#1324=FACE_OUTER_BOUND('',#1816,.T.);
#1325=FACE_OUTER_BOUND('',#1817,.T.);
#1326=FACE_OUTER_BOUND('',#1818,.T.);
#1327=FACE_OUTER_BOUND('',#1819,.T.);
#1328=FACE_OUTER_BOUND('',#1820,.T.);
#1329=FACE_OUTER_BOUND('',#1821,.T.);
#1330=FACE_OUTER_BOUND('',#1822,.T.);
#1331=FACE_OUTER_BOUND('',#1823,.T.);
#1332=FACE_OUTER_BOUND('',#1824,.T.);
#1333=FACE_OUTER_BOUND('',#1825,.T.);
#1334=FACE_OUTER_BOUND('',#1826,.T.);
#1335=FACE_OUTER_BOUND('',#1827,.T.);
#1336=FACE_OUTER_BOUND('',#1828,.T.);
#1337=FACE_OUTER_BOUND('',#1829,.T.);
#1338=FACE_OUTER_BOUND('',#1830,.T.);
#1339=FACE_OUTER_BOUND('',#1831,.T.);
#1340=FACE_OUTER_BOUND('',#1832,.T.);
#1341=FACE_OUTER_BOUND('',#1833,.T.);
#1342=FACE_OUTER_BOUND('',#1834,.T.);
#1343=FACE_OUTER_BOUND('',#1835,.T.);
#1344=FACE_OUTER_BOUND('',#1836,.T.);
#1345=FACE_OUTER_BOUND('',#1837,.T.);
#1346=FACE_OUTER_BOUND('',#1838,.T.);
#1347=FACE_OUTER_BOUND('',#1839,.T.);
#1348=FACE_OUTER_BOUND('',#1840,.T.);
#1349=FACE_OUTER_BOUND('',#1841,.T.);
#1350=FACE_OUTER_BOUND('',#1843,.T.);
#1351=FACE_OUTER_BOUND('',#1844,.T.);
#1352=FACE_OUTER_BOUND('',#1846,.T.);
#1353=FACE_OUTER_BOUND('',#1847,.T.);
#1354=FACE_OUTER_BOUND('',#1849,.T.);
#1355=FACE_OUTER_BOUND('',#1850,.T.);
#1356=FACE_OUTER_BOUND('',#1852,.T.);
#1357=FACE_OUTER_BOUND('',#1853,.T.);
#1358=FACE_OUTER_BOUND('',#1855,.T.);
#1359=FACE_OUTER_BOUND('',#1856,.T.);
#1360=FACE_OUTER_BOUND('',#1857,.T.);
#1361=FACE_OUTER_BOUND('',#1858,.T.);
#1362=FACE_OUTER_BOUND('',#1860,.T.);
#1363=FACE_OUTER_BOUND('',#1862,.T.);
#1364=FACE_OUTER_BOUND('',#1863,.T.);
#1365=FACE_OUTER_BOUND('',#1864,.T.);
#1366=FACE_OUTER_BOUND('',#1865,.T.);
#1367=FACE_OUTER_BOUND('',#1866,.T.);
#1368=FACE_OUTER_BOUND('',#1867,.T.);
#1369=FACE_OUTER_BOUND('',#1868,.T.);
#1370=FACE_OUTER_BOUND('',#1869,.T.);
#1371=FACE_OUTER_BOUND('',#1870,.T.);
#1372=FACE_OUTER_BOUND('',#1871,.T.);
#1373=FACE_OUTER_BOUND('',#1872,.T.);
#1374=FACE_OUTER_BOUND('',#1873,.T.);
#1375=FACE_OUTER_BOUND('',#1874,.T.);
#1376=FACE_OUTER_BOUND('',#1875,.T.);
#1377=FACE_OUTER_BOUND('',#1877,.T.);
#1378=FACE_OUTER_BOUND('',#1878,.T.);
#1379=FACE_OUTER_BOUND('',#1879,.T.);
#1380=FACE_OUTER_BOUND('',#1880,.T.);
#1381=FACE_OUTER_BOUND('',#1881,.T.);
#1382=FACE_OUTER_BOUND('',#1883,.T.);
#1383=FACE_OUTER_BOUND('',#1885,.T.);
#1384=FACE_OUTER_BOUND('',#1886,.T.);
#1385=FACE_OUTER_BOUND('',#1887,.T.);
#1386=FACE_OUTER_BOUND('',#1889,.T.);
#1387=FACE_OUTER_BOUND('',#1890,.T.);
#1388=FACE_OUTER_BOUND('',#1891,.T.);
#1389=FACE_OUTER_BOUND('',#1892,.T.);
#1390=FACE_OUTER_BOUND('',#1893,.T.);
#1391=FACE_OUTER_BOUND('',#1894,.T.);
#1392=FACE_OUTER_BOUND('',#1895,.T.);
#1393=FACE_OUTER_BOUND('',#1896,.T.);
#1394=FACE_OUTER_BOUND('',#1897,.T.);
#1395=FACE_OUTER_BOUND('',#1898,.T.);
#1396=FACE_OUTER_BOUND('',#1899,.T.);
#1397=FACE_OUTER_BOUND('',#1900,.T.);
#1398=FACE_OUTER_BOUND('',#1901,.T.);
#1399=FACE_OUTER_BOUND('',#1902,.T.);
#1400=FACE_OUTER_BOUND('',#1903,.T.);
#1401=FACE_OUTER_BOUND('',#1904,.T.);
#1402=FACE_OUTER_BOUND('',#1905,.T.);
#1403=FACE_OUTER_BOUND('',#1906,.T.);
#1404=FACE_OUTER_BOUND('',#1907,.T.);
#1405=FACE_OUTER_BOUND('',#1908,.T.);
#1406=FACE_OUTER_BOUND('',#1909,.T.);
#1407=FACE_OUTER_BOUND('',#1910,.T.);
#1408=FACE_OUTER_BOUND('',#1911,.T.);
#1409=FACE_OUTER_BOUND('',#1912,.T.);
#1410=FACE_OUTER_BOUND('',#1913,.T.);
#1411=FACE_OUTER_BOUND('',#1915,.T.);
#1412=FACE_OUTER_BOUND('',#1916,.T.);
#1413=FACE_OUTER_BOUND('',#1917,.T.);
#1414=FACE_OUTER_BOUND('',#1918,.T.);
#1415=FACE_OUTER_BOUND('',#1920,.T.);
#1416=FACE_OUTER_BOUND('',#1921,.T.);
#1417=FACE_OUTER_BOUND('',#1923,.T.);
#1418=FACE_OUTER_BOUND('',#1924,.T.);
#1419=FACE_OUTER_BOUND('',#1925,.T.);
#1420=FACE_OUTER_BOUND('',#1926,.T.);
#1421=FACE_OUTER_BOUND('',#1928,.T.);
#1422=FACE_OUTER_BOUND('',#1929,.T.);
#1423=FACE_OUTER_BOUND('',#1931,.T.);
#1424=FACE_OUTER_BOUND('',#1932,.T.);
#1425=FACE_OUTER_BOUND('',#1935,.T.);
#1426=EDGE_LOOP('',(#5202,#5203,#5204,#5205));
#1427=EDGE_LOOP('',(#5206,#5207,#5208,#5209));
#1428=EDGE_LOOP('',(#5210,#5211,#5212,#5213));
#1429=EDGE_LOOP('',(#5214,#5215,#5216,#5217));
#1430=EDGE_LOOP('',(#5218,#5219,#5220,#5221));
#1431=EDGE_LOOP('',(#5222));
#1432=EDGE_LOOP('',(#5223));
#1433=EDGE_LOOP('',(#5224));
#1434=EDGE_LOOP('',(#5225));
#1435=EDGE_LOOP('',(#5226,#5227,#5228,#5229));
#1436=EDGE_LOOP('',(#5230,#5231,#5232,#5233));
#1437=EDGE_LOOP('',(#5234));
#1438=EDGE_LOOP('',(#5235));
#1439=EDGE_LOOP('',(#5236));
#1440=EDGE_LOOP('',(#5237));
#1441=EDGE_LOOP('',(#5238,#5239,#5240,#5241));
#1442=EDGE_LOOP('',(#5242,#5243,#5244,#5245));
#1443=EDGE_LOOP('',(#5246,#5247,#5248,#5249));
#1444=EDGE_LOOP('',(#5250,#5251,#5252,#5253,#5254,#5255,#5256,#5257,#5258));
#1445=EDGE_LOOP('',(#5259,#5260));
#1446=EDGE_LOOP('',(#5261,#5262,#5263,#5264,#5265,#5266));
#1447=EDGE_LOOP('',(#5267,#5268,#5269,#5270));
#1448=EDGE_LOOP('',(#5271,#5272,#5273,#5274));
#1449=EDGE_LOOP('',(#5275,#5276,#5277,#5278));
#1450=EDGE_LOOP('',(#5279,#5280,#5281,#5282));
#1451=EDGE_LOOP('',(#5283,#5284,#5285,#5286));
#1452=EDGE_LOOP('',(#5287,#5288,#5289,#5290));
#1453=EDGE_LOOP('',(#5291,#5292,#5293,#5294));
#1454=EDGE_LOOP('',(#5295,#5296,#5297,#5298));
#1455=EDGE_LOOP('',(#5299,#5300,#5301,#5302));
#1456=EDGE_LOOP('',(#5303,#5304,#5305,#5306));
#1457=EDGE_LOOP('',(#5307,#5308,#5309,#5310));
#1458=EDGE_LOOP('',(#5311,#5312,#5313,#5314));
#1459=EDGE_LOOP('',(#5315,#5316,#5317,#5318));
#1460=EDGE_LOOP('',(#5319,#5320,#5321,#5322));
#1461=EDGE_LOOP('',(#5323));
#1462=EDGE_LOOP('',(#5324,#5325,#5326,#5327));
#1463=EDGE_LOOP('',(#5328,#5329,#5330,#5331));
#1464=EDGE_LOOP('',(#5332,#5333,#5334,#5335));
#1465=EDGE_LOOP('',(#5336,#5337,#5338,#5339));
#1466=EDGE_LOOP('',(#5340,#5341,#5342,#5343));
#1467=EDGE_LOOP('',(#5344,#5345,#5346,#5347));
#1468=EDGE_LOOP('',(#5348,#5349,#5350,#5351));
#1469=EDGE_LOOP('',(#5352,#5353,#5354,#5355));
#1470=EDGE_LOOP('',(#5356,#5357,#5358,#5359));
#1471=EDGE_LOOP('',(#5360,#5361,#5362,#5363));
#1472=EDGE_LOOP('',(#5364,#5365,#5366,#5367));
#1473=EDGE_LOOP('',(#5368,#5369,#5370,#5371));
#1474=EDGE_LOOP('',(#5372,#5373,#5374,#5375));
#1475=EDGE_LOOP('',(#5376,#5377,#5378,#5379));
#1476=EDGE_LOOP('',(#5380,#5381,#5382,#5383));
#1477=EDGE_LOOP('',(#5384,#5385,#5386,#5387));
#1478=EDGE_LOOP('',(#5388,#5389,#5390,#5391));
#1479=EDGE_LOOP('',(#5392,#5393,#5394,#5395));
#1480=EDGE_LOOP('',(#5396));
#1481=EDGE_LOOP('',(#5397,#5398,#5399,#5400));
#1482=EDGE_LOOP('',(#5401,#5402,#5403,#5404));
#1483=EDGE_LOOP('',(#5405,#5406,#5407,#5408));
#1484=EDGE_LOOP('',(#5409,#5410,#5411,#5412));
#1485=EDGE_LOOP('',(#5413,#5414,#5415,#5416,#5417));
#1486=EDGE_LOOP('',(#5418,#5419,#5420,#5421));
#1487=EDGE_LOOP('',(#5422,#5423,#5424,#5425));
#1488=EDGE_LOOP('',(#5426,#5427,#5428,#5429));
#1489=EDGE_LOOP('',(#5430,#5431,#5432,#5433));
#1490=EDGE_LOOP('',(#5434,#5435,#5436,#5437));
#1491=EDGE_LOOP('',(#5438,#5439,#5440,#5441));
#1492=EDGE_LOOP('',(#5442,#5443,#5444,#5445));
#1493=EDGE_LOOP('',(#5446,#5447,#5448,#5449));
#1494=EDGE_LOOP('',(#5450,#5451,#5452,#5453,#5454,#5455,#5456,#5457,#5458,
#5459,#5460,#5461,#5462,#5463,#5464,#5465,#5466,#5467,#5468,#5469,#5470,
#5471,#5472,#5473,#5474,#5475,#5476,#5477,#5478,#5479,#5480,#5481,#5482,
#5483,#5484,#5485,#5486,#5487,#5488,#5489,#5490,#5491,#5492,#5493));
#1495=EDGE_LOOP('',(#5494));
#1496=EDGE_LOOP('',(#5495,#5496,#5497,#5498,#5499,#5500,#5501,#5502,#5503,
#5504,#5505,#5506,#5507,#5508,#5509,#5510,#5511,#5512,#5513,#5514,#5515,
#5516,#5517,#5518,#5519,#5520,#5521,#5522,#5523,#5524,#5525,#5526,#5527,
#5528,#5529,#5530,#5531,#5532,#5533,#5534,#5535,#5536,#5537,#5538));
#1497=EDGE_LOOP('',(#5539));
#1498=EDGE_LOOP('',(#5540,#5541,#5542,#5543,#5544,#5545,#5546,#5547,#5548));
#1499=EDGE_LOOP('',(#5549,#5550));
#1500=EDGE_LOOP('',(#5551,#5552,#5553,#5554,#5555,#5556));
#1501=EDGE_LOOP('',(#5557,#5558,#5559,#5560));
#1502=EDGE_LOOP('',(#5561,#5562,#5563,#5564));
#1503=EDGE_LOOP('',(#5565,#5566,#5567,#5568));
#1504=EDGE_LOOP('',(#5569,#5570,#5571,#5572));
#1505=EDGE_LOOP('',(#5573,#5574,#5575,#5576));
#1506=EDGE_LOOP('',(#5577,#5578,#5579,#5580));
#1507=EDGE_LOOP('',(#5581,#5582,#5583,#5584));
#1508=EDGE_LOOP('',(#5585,#5586,#5587,#5588));
#1509=EDGE_LOOP('',(#5589,#5590,#5591,#5592));
#1510=EDGE_LOOP('',(#5593,#5594,#5595,#5596));
#1511=EDGE_LOOP('',(#5597,#5598,#5599,#5600));
#1512=EDGE_LOOP('',(#5601,#5602,#5603,#5604));
#1513=EDGE_LOOP('',(#5605,#5606,#5607,#5608));
#1514=EDGE_LOOP('',(#5609,#5610,#5611,#5612));
#1515=EDGE_LOOP('',(#5613));
#1516=EDGE_LOOP('',(#5614,#5615,#5616,#5617));
#1517=EDGE_LOOP('',(#5618,#5619,#5620,#5621));
#1518=EDGE_LOOP('',(#5622,#5623,#5624,#5625));
#1519=EDGE_LOOP('',(#5626,#5627,#5628,#5629));
#1520=EDGE_LOOP('',(#5630,#5631,#5632,#5633));
#1521=EDGE_LOOP('',(#5634,#5635,#5636,#5637));
#1522=EDGE_LOOP('',(#5638,#5639,#5640,#5641));
#1523=EDGE_LOOP('',(#5642,#5643,#5644,#5645));
#1524=EDGE_LOOP('',(#5646,#5647,#5648,#5649));
#1525=EDGE_LOOP('',(#5650,#5651,#5652,#5653));
#1526=EDGE_LOOP('',(#5654,#5655,#5656,#5657));
#1527=EDGE_LOOP('',(#5658,#5659,#5660,#5661));
#1528=EDGE_LOOP('',(#5662,#5663,#5664,#5665));
#1529=EDGE_LOOP('',(#5666,#5667,#5668,#5669));
#1530=EDGE_LOOP('',(#5670,#5671,#5672,#5673));
#1531=EDGE_LOOP('',(#5674,#5675,#5676,#5677));
#1532=EDGE_LOOP('',(#5678,#5679,#5680,#5681));
#1533=EDGE_LOOP('',(#5682,#5683,#5684,#5685));
#1534=EDGE_LOOP('',(#5686));
#1535=EDGE_LOOP('',(#5687,#5688,#5689,#5690));
#1536=EDGE_LOOP('',(#5691,#5692,#5693,#5694));
#1537=EDGE_LOOP('',(#5695,#5696,#5697,#5698));
#1538=EDGE_LOOP('',(#5699,#5700,#5701,#5702));
#1539=EDGE_LOOP('',(#5703,#5704,#5705,#5706,#5707));
#1540=EDGE_LOOP('',(#5708,#5709,#5710,#5711));
#1541=EDGE_LOOP('',(#5712,#5713,#5714,#5715));
#1542=EDGE_LOOP('',(#5716,#5717,#5718,#5719));
#1543=EDGE_LOOP('',(#5720,#5721,#5722,#5723));
#1544=EDGE_LOOP('',(#5724,#5725,#5726,#5727));
#1545=EDGE_LOOP('',(#5728,#5729,#5730,#5731));
#1546=EDGE_LOOP('',(#5732,#5733,#5734,#5735));
#1547=EDGE_LOOP('',(#5736,#5737,#5738,#5739));
#1548=EDGE_LOOP('',(#5740,#5741,#5742,#5743,#5744,#5745,#5746,#5747,#5748,
#5749,#5750,#5751,#5752,#5753,#5754,#5755,#5756,#5757,#5758,#5759,#5760,
#5761,#5762,#5763,#5764,#5765,#5766,#5767,#5768,#5769,#5770,#5771,#5772,
#5773,#5774,#5775,#5776,#5777,#5778,#5779,#5780,#5781,#5782,#5783));
#1549=EDGE_LOOP('',(#5784));
#1550=EDGE_LOOP('',(#5785,#5786,#5787,#5788,#5789,#5790,#5791,#5792,#5793,
#5794,#5795,#5796,#5797,#5798,#5799,#5800,#5801,#5802,#5803,#5804,#5805,
#5806,#5807,#5808,#5809,#5810,#5811,#5812,#5813,#5814,#5815,#5816,#5817,
#5818,#5819,#5820,#5821,#5822,#5823,#5824,#5825,#5826,#5827,#5828));
#1551=EDGE_LOOP('',(#5829));
#1552=EDGE_LOOP('',(#5830,#5831,#5832,#5833));
#1553=EDGE_LOOP('',(#5834,#5835,#5836,#5837));
#1554=EDGE_LOOP('',(#5838,#5839,#5840,#5841));
#1555=EDGE_LOOP('',(#5842,#5843,#5844,#5845));
#1556=EDGE_LOOP('',(#5846,#5847,#5848,#5849));
#1557=EDGE_LOOP('',(#5850,#5851,#5852,#5853));
#1558=EDGE_LOOP('',(#5854,#5855,#5856,#5857));
#1559=EDGE_LOOP('',(#5858,#5859,#5860,#5861));
#1560=EDGE_LOOP('',(#5862,#5863,#5864,#5865));
#1561=EDGE_LOOP('',(#5866,#5867,#5868,#5869));
#1562=EDGE_LOOP('',(#5870,#5871,#5872,#5873));
#1563=EDGE_LOOP('',(#5874,#5875,#5876,#5877));
#1564=EDGE_LOOP('',(#5878,#5879,#5880,#5881));
#1565=EDGE_LOOP('',(#5882,#5883,#5884,#5885));
#1566=EDGE_LOOP('',(#5886,#5887,#5888,#5889));
#1567=EDGE_LOOP('',(#5890,#5891,#5892,#5893));
#1568=EDGE_LOOP('',(#5894,#5895,#5896,#5897));
#1569=EDGE_LOOP('',(#5898,#5899,#5900,#5901));
#1570=EDGE_LOOP('',(#5902,#5903,#5904,#5905));
#1571=EDGE_LOOP('',(#5906,#5907,#5908,#5909));
#1572=EDGE_LOOP('',(#5910,#5911,#5912,#5913));
#1573=EDGE_LOOP('',(#5914,#5915,#5916,#5917));
#1574=EDGE_LOOP('',(#5918,#5919,#5920,#5921));
#1575=EDGE_LOOP('',(#5922,#5923,#5924,#5925));
#1576=EDGE_LOOP('',(#5926,#5927,#5928,#5929));
#1577=EDGE_LOOP('',(#5930,#5931,#5932,#5933));
#1578=EDGE_LOOP('',(#5934,#5935,#5936,#5937));
#1579=EDGE_LOOP('',(#5938,#5939,#5940,#5941));
#1580=EDGE_LOOP('',(#5942,#5943,#5944,#5945));
#1581=EDGE_LOOP('',(#5946,#5947,#5948,#5949));
#1582=EDGE_LOOP('',(#5950,#5951,#5952,#5953));
#1583=EDGE_LOOP('',(#5954,#5955,#5956,#5957));
#1584=EDGE_LOOP('',(#5958,#5959,#5960,#5961));
#1585=EDGE_LOOP('',(#5962,#5963,#5964,#5965));
#1586=EDGE_LOOP('',(#5966,#5967,#5968,#5969));
#1587=EDGE_LOOP('',(#5970,#5971,#5972,#5973));
#1588=EDGE_LOOP('',(#5974,#5975,#5976,#5977));
#1589=EDGE_LOOP('',(#5978,#5979,#5980,#5981));
#1590=EDGE_LOOP('',(#5982,#5983,#5984,#5985));
#1591=EDGE_LOOP('',(#5986,#5987,#5988,#5989));
#1592=EDGE_LOOP('',(#5990,#5991,#5992,#5993));
#1593=EDGE_LOOP('',(#5994,#5995,#5996,#5997));
#1594=EDGE_LOOP('',(#5998,#5999,#6000,#6001));
#1595=EDGE_LOOP('',(#6002,#6003,#6004,#6005));
#1596=EDGE_LOOP('',(#6006,#6007,#6008,#6009));
#1597=EDGE_LOOP('',(#6010,#6011,#6012,#6013,#6014,#6015,#6016,#6017,#6018,
#6019,#6020,#6021,#6022,#6023,#6024,#6025,#6026,#6027,#6028,#6029,#6030,
#6031,#6032,#6033,#6034,#6035,#6036,#6037,#6038,#6039,#6040,#6041,#6042,
#6043,#6044,#6045,#6046,#6047,#6048,#6049,#6050,#6051,#6052,#6053));
#1598=EDGE_LOOP('',(#6054));
#1599=EDGE_LOOP('',(#6055,#6056,#6057,#6058,#6059,#6060,#6061,#6062,#6063,
#6064,#6065,#6066,#6067,#6068,#6069,#6070,#6071,#6072,#6073,#6074,#6075,
#6076,#6077,#6078,#6079,#6080,#6081,#6082,#6083,#6084,#6085,#6086,#6087,
#6088,#6089,#6090,#6091,#6092,#6093,#6094,#6095,#6096,#6097,#6098));
#1600=EDGE_LOOP('',(#6099));
#1601=EDGE_LOOP('',(#6100,#6101,#6102,#6103));
#1602=EDGE_LOOP('',(#6104,#6105,#6106,#6107));
#1603=EDGE_LOOP('',(#6108,#6109,#6110,#6111));
#1604=EDGE_LOOP('',(#6112,#6113,#6114,#6115));
#1605=EDGE_LOOP('',(#6116,#6117,#6118,#6119));
#1606=EDGE_LOOP('',(#6120,#6121,#6122,#6123));
#1607=EDGE_LOOP('',(#6124,#6125,#6126,#6127,#6128,#6129));
#1608=EDGE_LOOP('',(#6130,#6131,#6132,#6133,#6134,#6135));
#1609=EDGE_LOOP('',(#6136));
#1610=EDGE_LOOP('',(#6137));
#1611=EDGE_LOOP('',(#6138,#6139,#6140,#6141));
#1612=EDGE_LOOP('',(#6142));
#1613=EDGE_LOOP('',(#6143));
#1614=EDGE_LOOP('',(#6144,#6145,#6146,#6147));
#1615=EDGE_LOOP('',(#6148,#6149,#6150,#6151));
#1616=EDGE_LOOP('',(#6152,#6153,#6154,#6155));
#1617=EDGE_LOOP('',(#6156));
#1618=EDGE_LOOP('',(#6157));
#1619=EDGE_LOOP('',(#6158,#6159,#6160,#6161));
#1620=EDGE_LOOP('',(#6162,#6163,#6164,#6165));
#1621=EDGE_LOOP('',(#6166));
#1622=EDGE_LOOP('',(#6167,#6168,#6169,#6170));
#1623=EDGE_LOOP('',(#6171,#6172,#6173,#6174));
#1624=EDGE_LOOP('',(#6175,#6176,#6177,#6178));
#1625=EDGE_LOOP('',(#6179));
#1626=EDGE_LOOP('',(#6180));
#1627=EDGE_LOOP('',(#6181,#6182,#6183,#6184));
#1628=EDGE_LOOP('',(#6185,#6186,#6187,#6188));
#1629=EDGE_LOOP('',(#6189,#6190,#6191,#6192));
#1630=EDGE_LOOP('',(#6193));
#1631=EDGE_LOOP('',(#6194,#6195,#6196,#6197));
#1632=EDGE_LOOP('',(#6198,#6199,#6200,#6201));
#1633=EDGE_LOOP('',(#6202,#6203,#6204,#6205));
#1634=EDGE_LOOP('',(#6206,#6207,#6208,#6209));
#1635=EDGE_LOOP('',(#6210,#6211,#6212,#6213));
#1636=EDGE_LOOP('',(#6214,#6215,#6216,#6217));
#1637=EDGE_LOOP('',(#6218,#6219,#6220,#6221,#6222,#6223));
#1638=EDGE_LOOP('',(#6224,#6225,#6226,#6227,#6228,#6229));
#1639=EDGE_LOOP('',(#6230,#6231,#6232,#6233));
#1640=EDGE_LOOP('',(#6234,#6235,#6236,#6237));
#1641=EDGE_LOOP('',(#6238,#6239,#6240,#6241));
#1642=EDGE_LOOP('',(#6242,#6243,#6244,#6245));
#1643=EDGE_LOOP('',(#6246,#6247,#6248,#6249));
#1644=EDGE_LOOP('',(#6250));
#1645=EDGE_LOOP('',(#6251));
#1646=EDGE_LOOP('',(#6252));
#1647=EDGE_LOOP('',(#6253));
#1648=EDGE_LOOP('',(#6254,#6255,#6256,#6257));
#1649=EDGE_LOOP('',(#6258,#6259,#6260,#6261));
#1650=EDGE_LOOP('',(#6262));
#1651=EDGE_LOOP('',(#6263));
#1652=EDGE_LOOP('',(#6264));
#1653=EDGE_LOOP('',(#6265));
#1654=EDGE_LOOP('',(#6266,#6267,#6268,#6269));
#1655=EDGE_LOOP('',(#6270,#6271,#6272,#6273));
#1656=EDGE_LOOP('',(#6274,#6275,#6276,#6277));
#1657=EDGE_LOOP('',(#6278,#6279,#6280,#6281));
#1658=EDGE_LOOP('',(#6282,#6283,#6284,#6285));
#1659=EDGE_LOOP('',(#6286));
#1660=EDGE_LOOP('',(#6287));
#1661=EDGE_LOOP('',(#6288,#6289,#6290,#6291));
#1662=EDGE_LOOP('',(#6292));
#1663=EDGE_LOOP('',(#6293));
#1664=EDGE_LOOP('',(#6294,#6295,#6296,#6297));
#1665=EDGE_LOOP('',(#6298,#6299,#6300,#6301));
#1666=EDGE_LOOP('',(#6302,#6303,#6304,#6305));
#1667=EDGE_LOOP('',(#6306,#6307,#6308,#6309));
#1668=EDGE_LOOP('',(#6310,#6311,#6312,#6313));
#1669=EDGE_LOOP('',(#6314,#6315,#6316,#6317));
#1670=EDGE_LOOP('',(#6318,#6319,#6320,#6321));
#1671=EDGE_LOOP('',(#6322));
#1672=EDGE_LOOP('',(#6323));
#1673=EDGE_LOOP('',(#6324,#6325,#6326,#6327));
#1674=EDGE_LOOP('',(#6328));
#1675=EDGE_LOOP('',(#6329));
#1676=EDGE_LOOP('',(#6330,#6331,#6332,#6333));
#1677=EDGE_LOOP('',(#6334,#6335,#6336,#6337));
#1678=EDGE_LOOP('',(#6338,#6339,#6340,#6341));
#1679=EDGE_LOOP('',(#6342,#6343,#6344,#6345));
#1680=EDGE_LOOP('',(#6346,#6347,#6348,#6349));
#1681=EDGE_LOOP('',(#6350,#6351,#6352,#6353));
#1682=EDGE_LOOP('',(#6354,#6355,#6356,#6357));
#1683=EDGE_LOOP('',(#6358,#6359,#6360,#6361));
#1684=EDGE_LOOP('',(#6362,#6363,#6364,#6365));
#1685=EDGE_LOOP('',(#6366,#6367,#6368,#6369));
#1686=EDGE_LOOP('',(#6370,#6371,#6372,#6373));
#1687=EDGE_LOOP('',(#6374,#6375,#6376,#6377));
#1688=EDGE_LOOP('',(#6378,#6379,#6380,#6381));
#1689=EDGE_LOOP('',(#6382,#6383,#6384,#6385));
#1690=EDGE_LOOP('',(#6386,#6387,#6388,#6389));
#1691=EDGE_LOOP('',(#6390,#6391,#6392,#6393));
#1692=EDGE_LOOP('',(#6394,#6395,#6396,#6397));
#1693=EDGE_LOOP('',(#6398,#6399,#6400,#6401));
#1694=EDGE_LOOP('',(#6402,#6403,#6404,#6405));
#1695=EDGE_LOOP('',(#6406));
#1696=EDGE_LOOP('',(#6407));
#1697=EDGE_LOOP('',(#6408,#6409,#6410,#6411));
#1698=EDGE_LOOP('',(#6412));
#1699=EDGE_LOOP('',(#6413));
#1700=EDGE_LOOP('',(#6414,#6415,#6416,#6417));
#1701=EDGE_LOOP('',(#6418,#6419,#6420,#6421));
#1702=EDGE_LOOP('',(#6422,#6423,#6424,#6425));
#1703=EDGE_LOOP('',(#6426,#6427,#6428,#6429));
#1704=EDGE_LOOP('',(#6430,#6431,#6432,#6433));
#1705=EDGE_LOOP('',(#6434,#6435,#6436,#6437));
#1706=EDGE_LOOP('',(#6438,#6439,#6440,#6441));
#1707=EDGE_LOOP('',(#6442,#6443,#6444,#6445));
#1708=EDGE_LOOP('',(#6446,#6447,#6448,#6449));
#1709=EDGE_LOOP('',(#6450,#6451,#6452,#6453));
#1710=EDGE_LOOP('',(#6454,#6455,#6456,#6457));
#1711=EDGE_LOOP('',(#6458,#6459,#6460,#6461));
#1712=EDGE_LOOP('',(#6462,#6463,#6464,#6465));
#1713=EDGE_LOOP('',(#6466,#6467,#6468,#6469));
#1714=EDGE_LOOP('',(#6470));
#1715=EDGE_LOOP('',(#6471));
#1716=EDGE_LOOP('',(#6472));
#1717=EDGE_LOOP('',(#6473));
#1718=EDGE_LOOP('',(#6474,#6475,#6476,#6477));
#1719=EDGE_LOOP('',(#6478));
#1720=EDGE_LOOP('',(#6479));
#1721=EDGE_LOOP('',(#6480,#6481,#6482,#6483));
#1722=EDGE_LOOP('',(#6484,#6485,#6486,#6487));
#1723=EDGE_LOOP('',(#6488));
#1724=EDGE_LOOP('',(#6489));
#1725=EDGE_LOOP('',(#6490));
#1726=EDGE_LOOP('',(#6491));
#1727=EDGE_LOOP('',(#6492,#6493,#6494,#6495));
#1728=EDGE_LOOP('',(#6496));
#1729=EDGE_LOOP('',(#6497));
#1730=EDGE_LOOP('',(#6498,#6499,#6500,#6501));
#1731=EDGE_LOOP('',(#6502,#6503,#6504,#6505));
#1732=EDGE_LOOP('',(#6506));
#1733=EDGE_LOOP('',(#6507));
#1734=EDGE_LOOP('',(#6508));
#1735=EDGE_LOOP('',(#6509));
#1736=EDGE_LOOP('',(#6510,#6511,#6512,#6513));
#1737=EDGE_LOOP('',(#6514));
#1738=EDGE_LOOP('',(#6515));
#1739=EDGE_LOOP('',(#6516,#6517,#6518,#6519));
#1740=EDGE_LOOP('',(#6520,#6521,#6522,#6523));
#1741=EDGE_LOOP('',(#6524));
#1742=EDGE_LOOP('',(#6525));
#1743=EDGE_LOOP('',(#6526));
#1744=EDGE_LOOP('',(#6527));
#1745=EDGE_LOOP('',(#6528,#6529,#6530,#6531));
#1746=EDGE_LOOP('',(#6532));
#1747=EDGE_LOOP('',(#6533));
#1748=EDGE_LOOP('',(#6534,#6535,#6536,#6537));
#1749=EDGE_LOOP('',(#6538,#6539,#6540,#6541));
#1750=EDGE_LOOP('',(#6542));
#1751=EDGE_LOOP('',(#6543));
#1752=EDGE_LOOP('',(#6544));
#1753=EDGE_LOOP('',(#6545));
#1754=EDGE_LOOP('',(#6546,#6547,#6548,#6549));
#1755=EDGE_LOOP('',(#6550));
#1756=EDGE_LOOP('',(#6551,#6552,#6553,#6554));
#1757=EDGE_LOOP('',(#6555));
#1758=EDGE_LOOP('',(#6556,#6557,#6558,#6559));
#1759=EDGE_LOOP('',(#6560));
#1760=EDGE_LOOP('',(#6561));
#1761=EDGE_LOOP('',(#6562));
#1762=EDGE_LOOP('',(#6563));
#1763=EDGE_LOOP('',(#6564,#6565,#6566,#6567));
#1764=EDGE_LOOP('',(#6568));
#1765=EDGE_LOOP('',(#6569));
#1766=EDGE_LOOP('',(#6570,#6571,#6572,#6573));
#1767=EDGE_LOOP('',(#6574));
#1768=EDGE_LOOP('',(#6575));
#1769=EDGE_LOOP('',(#6576,#6577,#6578,#6579));
#1770=EDGE_LOOP('',(#6580,#6581,#6582,#6583));
#1771=EDGE_LOOP('',(#6584,#6585,#6586,#6587));
#1772=EDGE_LOOP('',(#6588,#6589,#6590,#6591));
#1773=EDGE_LOOP('',(#6592));
#1774=EDGE_LOOP('',(#6593,#6594,#6595,#6596));
#1775=EDGE_LOOP('',(#6597,#6598,#6599,#6600));
#1776=EDGE_LOOP('',(#6601));
#1777=EDGE_LOOP('',(#6602,#6603,#6604,#6605));
#1778=EDGE_LOOP('',(#6606,#6607,#6608,#6609));
#1779=EDGE_LOOP('',(#6610));
#1780=EDGE_LOOP('',(#6611));
#1781=EDGE_LOOP('',(#6612,#6613,#6614,#6615));
#1782=EDGE_LOOP('',(#6616));
#1783=EDGE_LOOP('',(#6617));
#1784=EDGE_LOOP('',(#6618,#6619,#6620,#6621));
#1785=EDGE_LOOP('',(#6622,#6623,#6624,#6625));
#1786=EDGE_LOOP('',(#6626));
#1787=EDGE_LOOP('',(#6627));
#1788=EDGE_LOOP('',(#6628));
#1789=EDGE_LOOP('',(#6629));
#1790=EDGE_LOOP('',(#6630,#6631,#6632,#6633));
#1791=EDGE_LOOP('',(#6634,#6635,#6636,#6637));
#1792=EDGE_LOOP('',(#6638));
#1793=EDGE_LOOP('',(#6639));
#1794=EDGE_LOOP('',(#6640));
#1795=EDGE_LOOP('',(#6641));
#1796=EDGE_LOOP('',(#6642,#6643,#6644,#6645,#6646,#6647));
#1797=EDGE_LOOP('',(#6648,#6649,#6650,#6651,#6652));
#1798=EDGE_LOOP('',(#6653,#6654,#6655,#6656));
#1799=EDGE_LOOP('',(#6657,#6658,#6659,#6660));
#1800=EDGE_LOOP('',(#6661));
#1801=EDGE_LOOP('',(#6662));
#1802=EDGE_LOOP('',(#6663,#6664,#6665,#6666,#6667));
#1803=EDGE_LOOP('',(#6668));
#1804=EDGE_LOOP('',(#6669));
#1805=EDGE_LOOP('',(#6670,#6671,#6672,#6673));
#1806=EDGE_LOOP('',(#6674,#6675,#6676,#6677,#6678,#6679));
#1807=EDGE_LOOP('',(#6680,#6681,#6682,#6683,#6684));
#1808=EDGE_LOOP('',(#6685));
#1809=EDGE_LOOP('',(#6686));
#1810=EDGE_LOOP('',(#6687,#6688,#6689,#6690));
#1811=EDGE_LOOP('',(#6691,#6692,#6693,#6694));
#1812=EDGE_LOOP('',(#6695,#6696,#6697,#6698));
#1813=EDGE_LOOP('',(#6699));
#1814=EDGE_LOOP('',(#6700));
#1815=EDGE_LOOP('',(#6701,#6702,#6703,#6704,#6705));
#1816=EDGE_LOOP('',(#6706,#6707));
#1817=EDGE_LOOP('',(#6708,#6709));
#1818=EDGE_LOOP('',(#6710,#6711));
#1819=EDGE_LOOP('',(#6712,#6713));
#1820=EDGE_LOOP('',(#6714,#6715));
#1821=EDGE_LOOP('',(#6716,#6717));
#1822=EDGE_LOOP('',(#6718,#6719));
#1823=EDGE_LOOP('',(#6720,#6721));
#1824=EDGE_LOOP('',(#6722,#6723,#6724,#6725));
#1825=EDGE_LOOP('',(#6726,#6727,#6728,#6729,#6730,#6731,#6732,#6733,#6734,
#6735,#6736,#6737,#6738,#6739,#6740,#6741,#6742,#6743,#6744,#6745));
#1826=EDGE_LOOP('',(#6746,#6747,#6748,#6749));
#1827=EDGE_LOOP('',(#6750,#6751,#6752,#6753));
#1828=EDGE_LOOP('',(#6754,#6755,#6756,#6757));
#1829=EDGE_LOOP('',(#6758,#6759,#6760,#6761));
#1830=EDGE_LOOP('',(#6762,#6763,#6764,#6765));
#1831=EDGE_LOOP('',(#6766,#6767,#6768,#6769,#6770,#6771));
#1832=EDGE_LOOP('',(#6772,#6773,#6774,#6775));
#1833=EDGE_LOOP('',(#6776,#6777,#6778,#6779));
#1834=EDGE_LOOP('',(#6780,#6781,#6782,#6783));
#1835=EDGE_LOOP('',(#6784,#6785,#6786,#6787));
#1836=EDGE_LOOP('',(#6788,#6789,#6790,#6791));
#1837=EDGE_LOOP('',(#6792,#6793,#6794,#6795));
#1838=EDGE_LOOP('',(#6796,#6797,#6798,#6799,#6800,#6801,#6802,#6803,#6804,
#6805,#6806,#6807,#6808,#6809,#6810,#6811,#6812,#6813,#6814,#6815));
#1839=EDGE_LOOP('',(#6816,#6817,#6818,#6819));
#1840=EDGE_LOOP('',(#6820,#6821,#6822,#6823));
#1841=EDGE_LOOP('',(#6824));
#1842=EDGE_LOOP('',(#6825));
#1843=EDGE_LOOP('',(#6826,#6827,#6828,#6829));
#1844=EDGE_LOOP('',(#6830));
#1845=EDGE_LOOP('',(#6831));
#1846=EDGE_LOOP('',(#6832,#6833,#6834,#6835));
#1847=EDGE_LOOP('',(#6836));
#1848=EDGE_LOOP('',(#6837));
#1849=EDGE_LOOP('',(#6838,#6839,#6840,#6841));
#1850=EDGE_LOOP('',(#6842));
#1851=EDGE_LOOP('',(#6843));
#1852=EDGE_LOOP('',(#6844,#6845,#6846,#6847));
#1853=EDGE_LOOP('',(#6848));
#1854=EDGE_LOOP('',(#6849));
#1855=EDGE_LOOP('',(#6850,#6851,#6852,#6853));
#1856=EDGE_LOOP('',(#6854,#6855,#6856,#6857));
#1857=EDGE_LOOP('',(#6858,#6859,#6860,#6861));
#1858=EDGE_LOOP('',(#6862));
#1859=EDGE_LOOP('',(#6863));
#1860=EDGE_LOOP('',(#6864));
#1861=EDGE_LOOP('',(#6865));
#1862=EDGE_LOOP('',(#6866,#6867,#6868,#6869));
#1863=EDGE_LOOP('',(#6870,#6871,#6872,#6873));
#1864=EDGE_LOOP('',(#6874,#6875,#6876,#6877));
#1865=EDGE_LOOP('',(#6878,#6879,#6880,#6881));
#1866=EDGE_LOOP('',(#6882,#6883,#6884,#6885));
#1867=EDGE_LOOP('',(#6886,#6887,#6888,#6889));
#1868=EDGE_LOOP('',(#6890,#6891,#6892,#6893,#6894,#6895));
#1869=EDGE_LOOP('',(#6896,#6897,#6898,#6899,#6900,#6901));
#1870=EDGE_LOOP('',(#6902));
#1871=EDGE_LOOP('',(#6903));
#1872=EDGE_LOOP('',(#6904,#6905,#6906,#6907));
#1873=EDGE_LOOP('',(#6908,#6909,#6910,#6911));
#1874=EDGE_LOOP('',(#6912,#6913,#6914,#6915));
#1875=EDGE_LOOP('',(#6916));
#1876=EDGE_LOOP('',(#6917));
#1877=EDGE_LOOP('',(#6918,#6919,#6920,#6921));
#1878=EDGE_LOOP('',(#6922,#6923,#6924,#6925));
#1879=EDGE_LOOP('',(#6926,#6927,#6928,#6929));
#1880=EDGE_LOOP('',(#6930,#6931,#6932,#6933));
#1881=EDGE_LOOP('',(#6934));
#1882=EDGE_LOOP('',(#6935));
#1883=EDGE_LOOP('',(#6936));
#1884=EDGE_LOOP('',(#6937));
#1885=EDGE_LOOP('',(#6938,#6939,#6940,#6941));
#1886=EDGE_LOOP('',(#6942,#6943,#6944,#6945));
#1887=EDGE_LOOP('',(#6946,#6947,#6948,#6949));
#1888=EDGE_LOOP('',(#6950));
#1889=EDGE_LOOP('',(#6951,#6952,#6953,#6954,#6955,#6956,#6957,#6958,#6959,
#6960));
#1890=EDGE_LOOP('',(#6961,#6962,#6963,#6964));
#1891=EDGE_LOOP('',(#6965,#6966,#6967,#6968));
#1892=EDGE_LOOP('',(#6969,#6970,#6971,#6972,#6973,#6974,#6975,#6976,#6977,
#6978));
#1893=EDGE_LOOP('',(#6979,#6980,#6981,#6982));
#1894=EDGE_LOOP('',(#6983,#6984,#6985,#6986,#6987,#6988));
#1895=EDGE_LOOP('',(#6989,#6990,#6991,#6992,#6993,#6994,#6995,#6996));
#1896=EDGE_LOOP('',(#6997,#6998,#6999,#7000,#7001));
#1897=EDGE_LOOP('',(#7002,#7003,#7004,#7005));
#1898=EDGE_LOOP('',(#7006,#7007,#7008,#7009,#7010,#7011));
#1899=EDGE_LOOP('',(#7012,#7013,#7014,#7015));
#1900=EDGE_LOOP('',(#7016,#7017,#7018,#7019));
#1901=EDGE_LOOP('',(#7020,#7021,#7022,#7023));
#1902=EDGE_LOOP('',(#7024,#7025,#7026,#7027));
#1903=EDGE_LOOP('',(#7028,#7029,#7030,#7031));
#1904=EDGE_LOOP('',(#7032,#7033,#7034,#7035));
#1905=EDGE_LOOP('',(#7036,#7037,#7038,#7039));
#1906=EDGE_LOOP('',(#7040,#7041,#7042,#7043,#7044,#7045));
#1907=EDGE_LOOP('',(#7046,#7047,#7048,#7049,#7050,#7051));
#1908=EDGE_LOOP('',(#7052));
#1909=EDGE_LOOP('',(#7053));
#1910=EDGE_LOOP('',(#7054,#7055,#7056,#7057));
#1911=EDGE_LOOP('',(#7058,#7059,#7060,#7061));
#1912=EDGE_LOOP('',(#7062,#7063,#7064,#7065));
#1913=EDGE_LOOP('',(#7066));
#1914=EDGE_LOOP('',(#7067));
#1915=EDGE_LOOP('',(#7068,#7069,#7070,#7071));
#1916=EDGE_LOOP('',(#7072,#7073,#7074,#7075));
#1917=EDGE_LOOP('',(#7076,#7077,#7078,#7079));
#1918=EDGE_LOOP('',(#7080));
#1919=EDGE_LOOP('',(#7081));
#1920=EDGE_LOOP('',(#7082,#7083,#7084,#7085));
#1921=EDGE_LOOP('',(#7086));
#1922=EDGE_LOOP('',(#7087));
#1923=EDGE_LOOP('',(#7088,#7089,#7090,#7091));
#1924=EDGE_LOOP('',(#7092,#7093,#7094,#7095));
#1925=EDGE_LOOP('',(#7096,#7097,#7098,#7099));
#1926=EDGE_LOOP('',(#7100,#7101,#7102,#7103));
#1927=EDGE_LOOP('',(#7104));
#1928=EDGE_LOOP('',(#7105,#7106,#7107,#7108));
#1929=EDGE_LOOP('',(#7109,#7110,#7111,#7112));
#1930=EDGE_LOOP('',(#7113));
#1931=EDGE_LOOP('',(#7114,#7115,#7116,#7117));
#1932=EDGE_LOOP('',(#7118,#7119,#7120,#7121));
#1933=EDGE_LOOP('',(#7122));
#1934=EDGE_LOOP('',(#7123));
#1935=EDGE_LOOP('',(#7124,#7125,#7126,#7127));
#1936=EDGE_LOOP('',(#7128));
#1937=EDGE_LOOP('',(#7129));
#1938=LINE('',#11080,#2656);
#1939=LINE('',#11086,#2657);
#1940=LINE('',#11092,#2658);
#1941=LINE('',#11098,#2659);
#1942=LINE('',#11103,#2660);
#1943=LINE('',#11105,#2661);
#1944=LINE('',#11107,#2662);
#1945=LINE('',#11108,#2663);
#1946=LINE('',#11111,#2664);
#1947=LINE('',#11113,#2665);
#1948=LINE('',#11114,#2666);
#1949=LINE('',#11117,#2667);
#1950=LINE('',#11119,#2668);
#1951=LINE('',#11120,#2669);
#1952=LINE('',#11122,#2670);
#1953=LINE('',#11123,#2671);
#1954=LINE('',#11131,#2672);
#1955=LINE('',#11156,#2673);
#1956=LINE('',#11232,#2674);
#1957=LINE('',#11236,#2675);
#1958=LINE('',#11238,#2676);
#1959=LINE('',#11240,#2677);
#1960=LINE('',#11241,#2678);
#1961=LINE('',#11244,#2679);
#1962=LINE('',#11246,#2680);
#1963=LINE('',#11247,#2681);
#1964=LINE('',#11250,#2682);
#1965=LINE('',#11252,#2683);
#1966=LINE('',#11253,#2684);
#1967=LINE('',#11256,#2685);
#1968=LINE('',#11258,#2686);
#1969=LINE('',#11259,#2687);
#1970=LINE('',#11262,#2688);
#1971=LINE('',#11264,#2689);
#1972=LINE('',#11265,#2690);
#1973=LINE('',#11268,#2691);
#1974=LINE('',#11270,#2692);
#1975=LINE('',#11271,#2693);
#1976=LINE('',#11274,#2694);
#1977=LINE('',#11276,#2695);
#1978=LINE('',#11277,#2696);
#1979=LINE('',#11280,#2697);
#1980=LINE('',#11282,#2698);
#1981=LINE('',#11283,#2699);
#1982=LINE('',#11286,#2700);
#1983=LINE('',#11288,#2701);
#1984=LINE('',#11289,#2702);
#1985=LINE('',#11293,#2703);
#1986=LINE('',#11295,#2704);
#1987=LINE('',#11297,#2705);
#1988=LINE('',#11298,#2706);
#1989=LINE('',#11301,#2707);
#1990=LINE('',#11303,#2708);
#1991=LINE('',#11304,#2709);
#1992=LINE('',#11307,#2710);
#1993=LINE('',#11309,#2711);
#1994=LINE('',#11310,#2712);
#1995=LINE('',#11313,#2713);
#1996=LINE('',#11315,#2714);
#1997=LINE('',#11316,#2715);
#1998=LINE('',#11319,#2716);
#1999=LINE('',#11321,#2717);
#2000=LINE('',#11322,#2718);
#2001=LINE('',#11325,#2719);
#2002=LINE('',#11327,#2720);
#2003=LINE('',#11328,#2721);
#2004=LINE('',#11331,#2722);
#2005=LINE('',#11333,#2723);
#2006=LINE('',#11334,#2724);
#2007=LINE('',#11337,#2725);
#2008=LINE('',#11339,#2726);
#2009=LINE('',#11340,#2727);
#2010=LINE('',#11343,#2728);
#2011=LINE('',#11345,#2729);
#2012=LINE('',#11346,#2730);
#2013=LINE('',#11350,#2731);
#2014=LINE('',#11352,#2732);
#2015=LINE('',#11354,#2733);
#2016=LINE('',#11355,#2734);
#2017=LINE('',#11358,#2735);
#2018=LINE('',#11360,#2736);
#2019=LINE('',#11361,#2737);
#2020=LINE('',#11364,#2738);
#2021=LINE('',#11366,#2739);
#2022=LINE('',#11367,#2740);
#2023=LINE('',#11370,#2741);
#2024=LINE('',#11372,#2742);
#2025=LINE('',#11373,#2743);
#2026=LINE('',#11376,#2744);
#2027=LINE('',#11378,#2745);
#2028=LINE('',#11379,#2746);
#2029=LINE('',#11382,#2747);
#2030=LINE('',#11384,#2748);
#2031=LINE('',#11385,#2749);
#2032=LINE('',#11388,#2750);
#2033=LINE('',#11390,#2751);
#2034=LINE('',#11391,#2752);
#2035=LINE('',#11394,#2753);
#2036=LINE('',#11396,#2754);
#2037=LINE('',#11397,#2755);
#2038=LINE('',#11400,#2756);
#2039=LINE('',#11402,#2757);
#2040=LINE('',#11403,#2758);
#2041=LINE('',#11407,#2759);
#2042=LINE('',#11409,#2760);
#2043=LINE('',#11411,#2761);
#2044=LINE('',#11412,#2762);
#2045=LINE('',#11415,#2763);
#2046=LINE('',#11417,#2764);
#2047=LINE('',#11418,#2765);
#2048=LINE('',#11421,#2766);
#2049=LINE('',#11423,#2767);
#2050=LINE('',#11424,#2768);
#2051=LINE('',#11427,#2769);
#2052=LINE('',#11429,#2770);
#2053=LINE('',#11430,#2771);
#2054=LINE('',#11433,#2772);
#2055=LINE('',#11435,#2773);
#2056=LINE('',#11436,#2774);
#2057=LINE('',#11439,#2775);
#2058=LINE('',#11441,#2776);
#2059=LINE('',#11442,#2777);
#2060=LINE('',#11445,#2778);
#2061=LINE('',#11447,#2779);
#2062=LINE('',#11448,#2780);
#2063=LINE('',#11451,#2781);
#2064=LINE('',#11453,#2782);
#2065=LINE('',#11454,#2783);
#2066=LINE('',#11457,#2784);
#2067=LINE('',#11459,#2785);
#2068=LINE('',#11460,#2786);
#2069=LINE('',#11463,#2787);
#2070=LINE('',#11467,#2788);
#2071=LINE('',#11469,#2789);
#2072=LINE('',#11470,#2790);
#2073=LINE('',#11473,#2791);
#2074=LINE('',#11475,#2792);
#2075=LINE('',#11476,#2793);
#2076=LINE('',#11478,#2794);
#2077=LINE('',#11479,#2795);
#2078=LINE('',#11482,#2796);
#2079=LINE('',#11484,#2797);
#2080=LINE('',#11485,#2798);
#2081=LINE('',#11487,#2799);
#2082=LINE('',#11488,#2800);
#2083=LINE('',#11491,#2801);
#2084=LINE('',#11493,#2802);
#2085=LINE('',#11494,#2803);
#2086=LINE('',#11496,#2804);
#2087=LINE('',#11497,#2805);
#2088=LINE('',#11499,#2806);
#2089=LINE('',#11500,#2807);
#2090=LINE('',#11508,#2808);
#2091=LINE('',#11533,#2809);
#2092=LINE('',#11609,#2810);
#2093=LINE('',#11613,#2811);
#2094=LINE('',#11615,#2812);
#2095=LINE('',#11617,#2813);
#2096=LINE('',#11618,#2814);
#2097=LINE('',#11621,#2815);
#2098=LINE('',#11623,#2816);
#2099=LINE('',#11624,#2817);
#2100=LINE('',#11627,#2818);
#2101=LINE('',#11629,#2819);
#2102=LINE('',#11630,#2820);
#2103=LINE('',#11633,#2821);
#2104=LINE('',#11635,#2822);
#2105=LINE('',#11636,#2823);
#2106=LINE('',#11639,#2824);
#2107=LINE('',#11641,#2825);
#2108=LINE('',#11642,#2826);
#2109=LINE('',#11645,#2827);
#2110=LINE('',#11647,#2828);
#2111=LINE('',#11648,#2829);
#2112=LINE('',#11651,#2830);
#2113=LINE('',#11653,#2831);
#2114=LINE('',#11654,#2832);
#2115=LINE('',#11657,#2833);
#2116=LINE('',#11659,#2834);
#2117=LINE('',#11660,#2835);
#2118=LINE('',#11663,#2836);
#2119=LINE('',#11665,#2837);
#2120=LINE('',#11666,#2838);
#2121=LINE('',#11670,#2839);
#2122=LINE('',#11672,#2840);
#2123=LINE('',#11674,#2841);
#2124=LINE('',#11675,#2842);
#2125=LINE('',#11678,#2843);
#2126=LINE('',#11680,#2844);
#2127=LINE('',#11681,#2845);
#2128=LINE('',#11684,#2846);
#2129=LINE('',#11686,#2847);
#2130=LINE('',#11687,#2848);
#2131=LINE('',#11690,#2849);
#2132=LINE('',#11692,#2850);
#2133=LINE('',#11693,#2851);
#2134=LINE('',#11696,#2852);
#2135=LINE('',#11698,#2853);
#2136=LINE('',#11699,#2854);
#2137=LINE('',#11702,#2855);
#2138=LINE('',#11704,#2856);
#2139=LINE('',#11705,#2857);
#2140=LINE('',#11708,#2858);
#2141=LINE('',#11710,#2859);
#2142=LINE('',#11711,#2860);
#2143=LINE('',#11714,#2861);
#2144=LINE('',#11716,#2862);
#2145=LINE('',#11717,#2863);
#2146=LINE('',#11720,#2864);
#2147=LINE('',#11722,#2865);
#2148=LINE('',#11723,#2866);
#2149=LINE('',#11727,#2867);
#2150=LINE('',#11729,#2868);
#2151=LINE('',#11731,#2869);
#2152=LINE('',#11732,#2870);
#2153=LINE('',#11735,#2871);
#2154=LINE('',#11737,#2872);
#2155=LINE('',#11738,#2873);
#2156=LINE('',#11741,#2874);
#2157=LINE('',#11743,#2875);
#2158=LINE('',#11744,#2876);
#2159=LINE('',#11747,#2877);
#2160=LINE('',#11749,#2878);
#2161=LINE('',#11750,#2879);
#2162=LINE('',#11753,#2880);
#2163=LINE('',#11755,#2881);
#2164=LINE('',#11756,#2882);
#2165=LINE('',#11759,#2883);
#2166=LINE('',#11761,#2884);
#2167=LINE('',#11762,#2885);
#2168=LINE('',#11765,#2886);
#2169=LINE('',#11767,#2887);
#2170=LINE('',#11768,#2888);
#2171=LINE('',#11771,#2889);
#2172=LINE('',#11773,#2890);
#2173=LINE('',#11774,#2891);
#2174=LINE('',#11777,#2892);
#2175=LINE('',#11779,#2893);
#2176=LINE('',#11780,#2894);
#2177=LINE('',#11784,#2895);
#2178=LINE('',#11786,#2896);
#2179=LINE('',#11788,#2897);
#2180=LINE('',#11789,#2898);
#2181=LINE('',#11792,#2899);
#2182=LINE('',#11794,#2900);
#2183=LINE('',#11795,#2901);
#2184=LINE('',#11798,#2902);
#2185=LINE('',#11800,#2903);
#2186=LINE('',#11801,#2904);
#2187=LINE('',#11804,#2905);
#2188=LINE('',#11806,#2906);
#2189=LINE('',#11807,#2907);
#2190=LINE('',#11810,#2908);
#2191=LINE('',#11812,#2909);
#2192=LINE('',#11813,#2910);
#2193=LINE('',#11816,#2911);
#2194=LINE('',#11818,#2912);
#2195=LINE('',#11819,#2913);
#2196=LINE('',#11822,#2914);
#2197=LINE('',#11824,#2915);
#2198=LINE('',#11825,#2916);
#2199=LINE('',#11828,#2917);
#2200=LINE('',#11830,#2918);
#2201=LINE('',#11831,#2919);
#2202=LINE('',#11834,#2920);
#2203=LINE('',#11836,#2921);
#2204=LINE('',#11837,#2922);
#2205=LINE('',#11840,#2923);
#2206=LINE('',#11844,#2924);
#2207=LINE('',#11846,#2925);
#2208=LINE('',#11847,#2926);
#2209=LINE('',#11850,#2927);
#2210=LINE('',#11852,#2928);
#2211=LINE('',#11853,#2929);
#2212=LINE('',#11855,#2930);
#2213=LINE('',#11856,#2931);
#2214=LINE('',#11859,#2932);
#2215=LINE('',#11861,#2933);
#2216=LINE('',#11862,#2934);
#2217=LINE('',#11864,#2935);
#2218=LINE('',#11865,#2936);
#2219=LINE('',#11868,#2937);
#2220=LINE('',#11870,#2938);
#2221=LINE('',#11871,#2939);
#2222=LINE('',#11873,#2940);
#2223=LINE('',#11874,#2941);
#2224=LINE('',#11876,#2942);
#2225=LINE('',#11877,#2943);
#2226=LINE('',#11884,#2944);
#2227=LINE('',#11886,#2945);
#2228=LINE('',#11888,#2946);
#2229=LINE('',#11889,#2947);
#2230=LINE('',#11892,#2948);
#2231=LINE('',#11894,#2949);
#2232=LINE('',#11895,#2950);
#2233=LINE('',#11898,#2951);
#2234=LINE('',#11900,#2952);
#2235=LINE('',#11901,#2953);
#2236=LINE('',#11904,#2954);
#2237=LINE('',#11906,#2955);
#2238=LINE('',#11907,#2956);
#2239=LINE('',#11910,#2957);
#2240=LINE('',#11912,#2958);
#2241=LINE('',#11913,#2959);
#2242=LINE('',#11916,#2960);
#2243=LINE('',#11918,#2961);
#2244=LINE('',#11919,#2962);
#2245=LINE('',#11922,#2963);
#2246=LINE('',#11924,#2964);
#2247=LINE('',#11925,#2965);
#2248=LINE('',#11928,#2966);
#2249=LINE('',#11930,#2967);
#2250=LINE('',#11931,#2968);
#2251=LINE('',#11934,#2969);
#2252=LINE('',#11936,#2970);
#2253=LINE('',#11937,#2971);
#2254=LINE('',#11941,#2972);
#2255=LINE('',#11943,#2973);
#2256=LINE('',#11945,#2974);
#2257=LINE('',#11946,#2975);
#2258=LINE('',#11949,#2976);
#2259=LINE('',#11951,#2977);
#2260=LINE('',#11952,#2978);
#2261=LINE('',#11955,#2979);
#2262=LINE('',#11957,#2980);
#2263=LINE('',#11958,#2981);
#2264=LINE('',#11961,#2982);
#2265=LINE('',#11963,#2983);
#2266=LINE('',#11964,#2984);
#2267=LINE('',#11967,#2985);
#2268=LINE('',#11969,#2986);
#2269=LINE('',#11970,#2987);
#2270=LINE('',#11973,#2988);
#2271=LINE('',#11975,#2989);
#2272=LINE('',#11976,#2990);
#2273=LINE('',#11979,#2991);
#2274=LINE('',#11981,#2992);
#2275=LINE('',#11982,#2993);
#2276=LINE('',#11985,#2994);
#2277=LINE('',#11987,#2995);
#2278=LINE('',#11988,#2996);
#2279=LINE('',#11991,#2997);
#2280=LINE('',#11993,#2998);
#2281=LINE('',#11994,#2999);
#2282=LINE('',#11998,#3000);
#2283=LINE('',#12000,#3001);
#2284=LINE('',#12002,#3002);
#2285=LINE('',#12003,#3003);
#2286=LINE('',#12006,#3004);
#2287=LINE('',#12008,#3005);
#2288=LINE('',#12009,#3006);
#2289=LINE('',#12012,#3007);
#2290=LINE('',#12014,#3008);
#2291=LINE('',#12015,#3009);
#2292=LINE('',#12018,#3010);
#2293=LINE('',#12020,#3011);
#2294=LINE('',#12021,#3012);
#2295=LINE('',#12024,#3013);
#2296=LINE('',#12026,#3014);
#2297=LINE('',#12027,#3015);
#2298=LINE('',#12030,#3016);
#2299=LINE('',#12032,#3017);
#2300=LINE('',#12033,#3018);
#2301=LINE('',#12036,#3019);
#2302=LINE('',#12038,#3020);
#2303=LINE('',#12039,#3021);
#2304=LINE('',#12042,#3022);
#2305=LINE('',#12044,#3023);
#2306=LINE('',#12045,#3024);
#2307=LINE('',#12048,#3025);
#2308=LINE('',#12050,#3026);
#2309=LINE('',#12051,#3027);
#2310=LINE('',#12055,#3028);
#2311=LINE('',#12057,#3029);
#2312=LINE('',#12059,#3030);
#2313=LINE('',#12060,#3031);
#2314=LINE('',#12063,#3032);
#2315=LINE('',#12065,#3033);
#2316=LINE('',#12066,#3034);
#2317=LINE('',#12069,#3035);
#2318=LINE('',#12071,#3036);
#2319=LINE('',#12072,#3037);
#2320=LINE('',#12075,#3038);
#2321=LINE('',#12077,#3039);
#2322=LINE('',#12078,#3040);
#2323=LINE('',#12081,#3041);
#2324=LINE('',#12083,#3042);
#2325=LINE('',#12084,#3043);
#2326=LINE('',#12087,#3044);
#2327=LINE('',#12089,#3045);
#2328=LINE('',#12090,#3046);
#2329=LINE('',#12093,#3047);
#2330=LINE('',#12095,#3048);
#2331=LINE('',#12096,#3049);
#2332=LINE('',#12099,#3050);
#2333=LINE('',#12101,#3051);
#2334=LINE('',#12102,#3052);
#2335=LINE('',#12105,#3053);
#2336=LINE('',#12107,#3054);
#2337=LINE('',#12108,#3055);
#2338=LINE('',#12113,#3056);
#2339=LINE('',#12117,#3057);
#2340=LINE('',#12119,#3058);
#2341=LINE('',#12120,#3059);
#2342=LINE('',#12123,#3060);
#2343=LINE('',#12125,#3061);
#2344=LINE('',#12126,#3062);
#2345=LINE('',#12128,#3063);
#2346=LINE('',#12129,#3064);
#2347=LINE('',#12132,#3065);
#2348=LINE('',#12134,#3066);
#2349=LINE('',#12135,#3067);
#2350=LINE('',#12137,#3068);
#2351=LINE('',#12138,#3069);
#2352=LINE('',#12141,#3070);
#2353=LINE('',#12143,#3071);
#2354=LINE('',#12144,#3072);
#2355=LINE('',#12146,#3073);
#2356=LINE('',#12147,#3074);
#2357=LINE('',#12149,#3075);
#2358=LINE('',#12150,#3076);
#2359=LINE('',#12157,#3077);
#2360=LINE('',#12159,#3078);
#2361=LINE('',#12161,#3079);
#2362=LINE('',#12162,#3080);
#2363=LINE('',#12165,#3081);
#2364=LINE('',#12167,#3082);
#2365=LINE('',#12168,#3083);
#2366=LINE('',#12171,#3084);
#2367=LINE('',#12173,#3085);
#2368=LINE('',#12174,#3086);
#2369=LINE('',#12177,#3087);
#2370=LINE('',#12179,#3088);
#2371=LINE('',#12180,#3089);
#2372=LINE('',#12183,#3090);
#2373=LINE('',#12185,#3091);
#2374=LINE('',#12186,#3092);
#2375=LINE('',#12188,#3093);
#2376=LINE('',#12189,#3094);
#2377=LINE('',#12199,#3095);
#2378=LINE('',#12208,#3096);
#2379=LINE('',#12212,#3097);
#2380=LINE('',#12216,#3098);
#2381=LINE('',#12223,#3099);
#2382=LINE('',#12225,#3100);
#2383=LINE('',#12233,#3101);
#2384=LINE('',#12237,#3102);
#2385=LINE('',#12241,#3103);
#2386=LINE('',#12248,#3104);
#2387=LINE('',#12252,#3105);
#2388=LINE('',#12256,#3106);
#2389=LINE('',#12261,#3107);
#2390=LINE('',#12263,#3108);
#2391=LINE('',#12265,#3109);
#2392=LINE('',#12266,#3110);
#2393=LINE('',#12269,#3111);
#2394=LINE('',#12271,#3112);
#2395=LINE('',#12272,#3113);
#2396=LINE('',#12275,#3114);
#2397=LINE('',#12277,#3115);
#2398=LINE('',#12278,#3116);
#2399=LINE('',#12281,#3117);
#2400=LINE('',#12283,#3118);
#2401=LINE('',#12284,#3119);
#2402=LINE('',#12287,#3120);
#2403=LINE('',#12289,#3121);
#2404=LINE('',#12290,#3122);
#2405=LINE('',#12292,#3123);
#2406=LINE('',#12293,#3124);
#2407=LINE('',#12301,#3125);
#2408=LINE('',#12307,#3126);
#2409=LINE('',#12313,#3127);
#2410=LINE('',#12319,#3128);
#2411=LINE('',#12324,#3129);
#2412=LINE('',#12326,#3130);
#2413=LINE('',#12328,#3131);
#2414=LINE('',#12329,#3132);
#2415=LINE('',#12332,#3133);
#2416=LINE('',#12334,#3134);
#2417=LINE('',#12335,#3135);
#2418=LINE('',#12338,#3136);
#2419=LINE('',#12340,#3137);
#2420=LINE('',#12341,#3138);
#2421=LINE('',#12343,#3139);
#2422=LINE('',#12344,#3140);
#2423=LINE('',#12352,#3141);
#2424=LINE('',#12356,#3142);
#2425=LINE('',#12363,#3143);
#2426=LINE('',#12371,#3144);
#2427=LINE('',#12377,#3145);
#2428=LINE('',#12382,#3146);
#2429=LINE('',#12384,#3147);
#2430=LINE('',#12386,#3148);
#2431=LINE('',#12387,#3149);
#2432=LINE('',#12390,#3150);
#2433=LINE('',#12392,#3151);
#2434=LINE('',#12393,#3152);
#2435=LINE('',#12396,#3153);
#2436=LINE('',#12398,#3154);
#2437=LINE('',#12399,#3155);
#2438=LINE('',#12401,#3156);
#2439=LINE('',#12402,#3157);
#2440=LINE('',#12409,#3158);
#2441=LINE('',#12411,#3159);
#2442=LINE('',#12413,#3160);
#2443=LINE('',#12414,#3161);
#2444=LINE('',#12417,#3162);
#2445=LINE('',#12419,#3163);
#2446=LINE('',#12420,#3164);
#2447=LINE('',#12423,#3165);
#2448=LINE('',#12425,#3166);
#2449=LINE('',#12426,#3167);
#2450=LINE('',#12428,#3168);
#2451=LINE('',#12429,#3169);
#2452=LINE('',#12436,#3170);
#2453=LINE('',#12438,#3171);
#2454=LINE('',#12440,#3172);
#2455=LINE('',#12441,#3173);
#2456=LINE('',#12444,#3174);
#2457=LINE('',#12446,#3175);
#2458=LINE('',#12447,#3176);
#2459=LINE('',#12450,#3177);
#2460=LINE('',#12452,#3178);
#2461=LINE('',#12453,#3179);
#2462=LINE('',#12455,#3180);
#2463=LINE('',#12456,#3181);
#2464=LINE('',#12464,#3182);
#2465=LINE('',#12470,#3183);
#2466=LINE('',#12475,#3184);
#2467=LINE('',#12477,#3185);
#2468=LINE('',#12479,#3186);
#2469=LINE('',#12480,#3187);
#2470=LINE('',#12483,#3188);
#2471=LINE('',#12485,#3189);
#2472=LINE('',#12486,#3190);
#2473=LINE('',#12489,#3191);
#2474=LINE('',#12491,#3192);
#2475=LINE('',#12492,#3193);
#2476=LINE('',#12494,#3194);
#2477=LINE('',#12495,#3195);
#2478=LINE('',#12502,#3196);
#2479=LINE('',#12504,#3197);
#2480=LINE('',#12506,#3198);
#2481=LINE('',#12507,#3199);
#2482=LINE('',#12510,#3200);
#2483=LINE('',#12512,#3201);
#2484=LINE('',#12513,#3202);
#2485=LINE('',#12516,#3203);
#2486=LINE('',#12518,#3204);
#2487=LINE('',#12519,#3205);
#2488=LINE('',#12521,#3206);
#2489=LINE('',#12522,#3207);
#2490=LINE('',#12529,#3208);
#2491=LINE('',#12531,#3209);
#2492=LINE('',#12533,#3210);
#2493=LINE('',#12534,#3211);
#2494=LINE('',#12537,#3212);
#2495=LINE('',#12539,#3213);
#2496=LINE('',#12540,#3214);
#2497=LINE('',#12543,#3215);
#2498=LINE('',#12545,#3216);
#2499=LINE('',#12546,#3217);
#2500=LINE('',#12548,#3218);
#2501=LINE('',#12549,#3219);
#2502=LINE('',#12558,#3220);
#2503=LINE('',#12564,#3221);
#2504=LINE('',#12573,#3222);
#2505=LINE('',#12580,#3223);
#2506=LINE('',#12586,#3224);
#2507=LINE('',#12595,#3225);
#2508=LINE('',#12602,#3226);
#2509=LINE('',#12608,#3227);
#2510=LINE('',#12617,#3228);
#2511=LINE('',#12625,#3229);
#2512=LINE('',#12630,#3230);
#2513=LINE('',#12639,#3231);
#2514=LINE('',#12647,#3232);
#2515=LINE('',#12652,#3233);
#2516=LINE('',#12661,#3234);
#2517=LINE('',#12668,#3235);
#2518=LINE('',#12675,#3236);
#2519=LINE('',#12684,#3237);
#2520=LINE('',#12693,#3238);
#2521=LINE('',#12701,#3239);
#2522=LINE('',#12705,#3240);
#2523=LINE('',#12710,#3241);
#2524=LINE('',#12715,#3242);
#2525=LINE('',#12717,#3243);
#2526=LINE('',#12719,#3244);
#2527=LINE('',#12720,#3245);
#2528=LINE('',#12723,#3246);
#2529=LINE('',#12725,#3247);
#2530=LINE('',#12726,#3248);
#2531=LINE('',#12729,#3249);
#2532=LINE('',#12731,#3250);
#2533=LINE('',#12732,#3251);
#2534=LINE('',#12734,#3252);
#2535=LINE('',#12735,#3253);
#2536=LINE('',#12743,#3254);
#2537=LINE('',#12749,#3255);
#2538=LINE('',#12758,#3256);
#2539=LINE('',#12764,#3257);
#2540=LINE('',#12782,#3258);
#2541=LINE('',#12788,#3259);
#2542=LINE('',#12792,#3260);
#2543=LINE('',#12798,#3261);
#2544=LINE('',#12803,#3262);
#2545=LINE('',#12818,#3263);
#2546=LINE('',#12827,#3264);
#2547=LINE('',#12831,#3265);
#2548=LINE('',#12835,#3266);
#2549=LINE('',#12838,#3267);
#2550=LINE('',#12991,#3268);
#2551=LINE('',#13287,#3269);
#2552=LINE('',#13329,#3270);
#2553=LINE('',#13334,#3271);
#2554=LINE('',#13343,#3272);
#2555=LINE('',#13348,#3273);
#2556=LINE('',#13359,#3274);
#2557=LINE('',#13365,#3275);
#2558=LINE('',#13373,#3276);
#2559=LINE('',#13375,#3277);
#2560=LINE('',#13377,#3278);
#2561=LINE('',#13378,#3279);
#2562=LINE('',#13381,#3280);
#2563=LINE('',#13383,#3281);
#2564=LINE('',#13384,#3282);
#2565=LINE('',#13387,#3283);
#2566=LINE('',#13389,#3284);
#2567=LINE('',#13390,#3285);
#2568=LINE('',#13393,#3286);
#2569=LINE('',#13395,#3287);
#2570=LINE('',#13396,#3288);
#2571=LINE('',#13399,#3289);
#2572=LINE('',#13401,#3290);
#2573=LINE('',#13402,#3291);
#2574=LINE('',#13404,#3292);
#2575=LINE('',#13405,#3293);
#2576=LINE('',#13417,#3294);
#2577=LINE('',#13421,#3295);
#2578=LINE('',#13425,#3296);
#2579=LINE('',#13432,#3297);
#2580=LINE('',#13434,#3298);
#2581=LINE('',#13440,#3299);
#2582=LINE('',#13446,#3300);
#2583=LINE('',#13454,#3301);
#2584=LINE('',#13456,#3302);
#2585=LINE('',#13458,#3303);
#2586=LINE('',#13459,#3304);
#2587=LINE('',#13462,#3305);
#2588=LINE('',#13464,#3306);
#2589=LINE('',#13465,#3307);
#2590=LINE('',#13468,#3308);
#2591=LINE('',#13470,#3309);
#2592=LINE('',#13471,#3310);
#2593=LINE('',#13476,#3311);
#2594=LINE('',#13478,#3312);
#2595=LINE('',#13480,#3313);
#2596=LINE('',#13482,#3314);
#2597=LINE('',#13484,#3315);
#2598=LINE('',#13486,#3316);
#2599=LINE('',#13487,#3317);
#2600=LINE('',#13490,#3318);
#2601=LINE('',#13491,#3319);
#2602=LINE('',#13494,#3320);
#2603=LINE('',#13495,#3321);
#2604=LINE('',#13498,#3322);
#2605=LINE('',#13500,#3323);
#2606=LINE('',#13502,#3324);
#2607=LINE('',#13504,#3325);
#2608=LINE('',#13505,#3326);
#2609=LINE('',#13507,#3327);
#2610=LINE('',#13510,#3328);
#2611=LINE('',#13513,#3329);
#2612=LINE('',#13517,#3330);
#2613=LINE('',#13524,#3331);
#2614=LINE('',#13526,#3332);
#2615=LINE('',#13528,#3333);
#2616=LINE('',#13534,#3334);
#2617=LINE('',#13536,#3335);
#2618=LINE('',#13538,#3336);
#2619=LINE('',#13539,#3337);
#2620=LINE('',#13542,#3338);
#2621=LINE('',#13544,#3339);
#2622=LINE('',#13545,#3340);
#2623=LINE('',#13548,#3341);
#2624=LINE('',#13550,#3342);
#2625=LINE('',#13551,#3343);
#2626=LINE('',#13554,#3344);
#2627=LINE('',#13556,#3345);
#2628=LINE('',#13557,#3346);
#2629=LINE('',#13560,#3347);
#2630=LINE('',#13562,#3348);
#2631=LINE('',#13563,#3349);
#2632=LINE('',#13565,#3350);
#2633=LINE('',#13566,#3351);
#2634=LINE('',#13578,#3352);
#2635=LINE('',#13582,#3353);
#2636=LINE('',#13586,#3354);
#2637=LINE('',#13593,#3355);
#2638=LINE('',#13595,#3356);
#2639=LINE('',#13657,#3357);
#2640=LINE('',#13666,#3358);
#2641=LINE('',#13674,#3359);
#2642=LINE('',#13678,#3360);
#2643=LINE('',#13683,#3361);
#2644=LINE('',#13688,#3362);
#2645=LINE('',#13690,#3363);
#2646=LINE('',#13692,#3364);
#2647=LINE('',#13693,#3365);
#2648=LINE('',#13696,#3366);
#2649=LINE('',#13698,#3367);
#2650=LINE('',#13699,#3368);
#2651=LINE('',#13702,#3369);
#2652=LINE('',#13704,#3370);
#2653=LINE('',#13705,#3371);
#2654=LINE('',#13707,#3372);
#2655=LINE('',#13708,#3373);
#2656=VECTOR('',#8827,0.274999999999999);
#2657=VECTOR('',#8834,0.274999999999999);
#2658=VECTOR('',#8841,0.274999999999999);
#2659=VECTOR('',#8848,0.274999999999999);
#2660=VECTOR('',#8853,1.);
#2661=VECTOR('',#8854,1.);
#2662=VECTOR('',#8855,1.);
#2663=VECTOR('',#8856,1.);
#2664=VECTOR('',#8859,1.);
#2665=VECTOR('',#8860,1.);
#2666=VECTOR('',#8861,1.);
#2667=VECTOR('',#8864,1.);
#2668=VECTOR('',#8865,1.);
#2669=VECTOR('',#8866,1.);
#2670=VECTOR('',#8869,1.);
#2671=VECTOR('',#8870,1.);
#2672=VECTOR('',#8881,0.275);
#2673=VECTOR('',#8882,0.275);
#2674=VECTOR('',#8889,0.21);
#2675=VECTOR('',#8892,1.);
#2676=VECTOR('',#8893,1.);
#2677=VECTOR('',#8894,1.);
#2678=VECTOR('',#8895,1.);
#2679=VECTOR('',#8898,1.);
#2680=VECTOR('',#8899,1.);
#2681=VECTOR('',#8900,1.);
#2682=VECTOR('',#8903,1.);
#2683=VECTOR('',#8904,1.);
#2684=VECTOR('',#8905,1.);
#2685=VECTOR('',#8908,1.);
#2686=VECTOR('',#8909,1.);
#2687=VECTOR('',#8910,1.);
#2688=VECTOR('',#8913,1.);
#2689=VECTOR('',#8914,1.);
#2690=VECTOR('',#8915,1.);
#2691=VECTOR('',#8918,1.);
#2692=VECTOR('',#8919,1.);
#2693=VECTOR('',#8920,1.);
#2694=VECTOR('',#8923,1.);
#2695=VECTOR('',#8924,1.);
#2696=VECTOR('',#8925,1.);
#2697=VECTOR('',#8928,1.);
#2698=VECTOR('',#8929,1.);
#2699=VECTOR('',#8930,1.);
#2700=VECTOR('',#8933,1.);
#2701=VECTOR('',#8934,1.);
#2702=VECTOR('',#8935,1.);
#2703=VECTOR('',#8938,1.);
#2704=VECTOR('',#8939,1.);
#2705=VECTOR('',#8940,1.);
#2706=VECTOR('',#8941,1.);
#2707=VECTOR('',#8944,1.);
#2708=VECTOR('',#8945,1.);
#2709=VECTOR('',#8946,1.);
#2710=VECTOR('',#8949,1.);
#2711=VECTOR('',#8950,1.);
#2712=VECTOR('',#8951,1.);
#2713=VECTOR('',#8954,1.);
#2714=VECTOR('',#8955,1.);
#2715=VECTOR('',#8956,1.);
#2716=VECTOR('',#8959,1.);
#2717=VECTOR('',#8960,1.);
#2718=VECTOR('',#8961,1.);
#2719=VECTOR('',#8964,1.);
#2720=VECTOR('',#8965,1.);
#2721=VECTOR('',#8966,1.);
#2722=VECTOR('',#8969,1.);
#2723=VECTOR('',#8970,1.);
#2724=VECTOR('',#8971,1.);
#2725=VECTOR('',#8974,1.);
#2726=VECTOR('',#8975,1.);
#2727=VECTOR('',#8976,1.);
#2728=VECTOR('',#8979,1.);
#2729=VECTOR('',#8980,1.);
#2730=VECTOR('',#8981,1.);
#2731=VECTOR('',#8984,1.);
#2732=VECTOR('',#8985,1.);
#2733=VECTOR('',#8986,1.);
#2734=VECTOR('',#8987,1.);
#2735=VECTOR('',#8990,1.);
#2736=VECTOR('',#8991,1.);
#2737=VECTOR('',#8992,1.);
#2738=VECTOR('',#8995,1.);
#2739=VECTOR('',#8996,1.);
#2740=VECTOR('',#8997,1.);
#2741=VECTOR('',#9000,1.);
#2742=VECTOR('',#9001,1.);
#2743=VECTOR('',#9002,1.);
#2744=VECTOR('',#9005,1.);
#2745=VECTOR('',#9006,1.);
#2746=VECTOR('',#9007,1.);
#2747=VECTOR('',#9010,1.);
#2748=VECTOR('',#9011,1.);
#2749=VECTOR('',#9012,1.);
#2750=VECTOR('',#9015,1.);
#2751=VECTOR('',#9016,1.);
#2752=VECTOR('',#9017,1.);
#2753=VECTOR('',#9020,1.);
#2754=VECTOR('',#9021,1.);
#2755=VECTOR('',#9022,1.);
#2756=VECTOR('',#9025,1.);
#2757=VECTOR('',#9026,1.);
#2758=VECTOR('',#9027,1.);
#2759=VECTOR('',#9030,1.);
#2760=VECTOR('',#9031,1.);
#2761=VECTOR('',#9032,1.);
#2762=VECTOR('',#9033,1.);
#2763=VECTOR('',#9036,1.);
#2764=VECTOR('',#9037,1.);
#2765=VECTOR('',#9038,1.);
#2766=VECTOR('',#9041,1.);
#2767=VECTOR('',#9042,1.);
#2768=VECTOR('',#9043,1.);
#2769=VECTOR('',#9046,1.);
#2770=VECTOR('',#9047,1.);
#2771=VECTOR('',#9048,1.);
#2772=VECTOR('',#9051,1.);
#2773=VECTOR('',#9052,1.);
#2774=VECTOR('',#9053,1.);
#2775=VECTOR('',#9056,1.);
#2776=VECTOR('',#9057,1.);
#2777=VECTOR('',#9058,1.);
#2778=VECTOR('',#9061,1.);
#2779=VECTOR('',#9062,1.);
#2780=VECTOR('',#9063,1.);
#2781=VECTOR('',#9066,1.);
#2782=VECTOR('',#9067,1.);
#2783=VECTOR('',#9068,1.);
#2784=VECTOR('',#9071,1.);
#2785=VECTOR('',#9072,1.);
#2786=VECTOR('',#9073,1.);
#2787=VECTOR('',#9076,0.21);
#2788=VECTOR('',#9081,1.);
#2789=VECTOR('',#9082,1.);
#2790=VECTOR('',#9083,1.);
#2791=VECTOR('',#9086,1.);
#2792=VECTOR('',#9087,1.);
#2793=VECTOR('',#9088,1.);
#2794=VECTOR('',#9091,1.);
#2795=VECTOR('',#9092,1.);
#2796=VECTOR('',#9095,1.);
#2797=VECTOR('',#9096,1.);
#2798=VECTOR('',#9097,1.);
#2799=VECTOR('',#9100,1.);
#2800=VECTOR('',#9101,1.);
#2801=VECTOR('',#9104,1.);
#2802=VECTOR('',#9105,1.);
#2803=VECTOR('',#9106,1.);
#2804=VECTOR('',#9109,1.);
#2805=VECTOR('',#9110,1.);
#2806=VECTOR('',#9113,1.);
#2807=VECTOR('',#9114,1.);
#2808=VECTOR('',#9125,0.275);
#2809=VECTOR('',#9126,0.275);
#2810=VECTOR('',#9133,0.21);
#2811=VECTOR('',#9136,1.);
#2812=VECTOR('',#9137,1.);
#2813=VECTOR('',#9138,1.);
#2814=VECTOR('',#9139,1.);
#2815=VECTOR('',#9142,1.);
#2816=VECTOR('',#9143,1.);
#2817=VECTOR('',#9144,1.);
#2818=VECTOR('',#9147,1.);
#2819=VECTOR('',#9148,1.);
#2820=VECTOR('',#9149,1.);
#2821=VECTOR('',#9152,1.);
#2822=VECTOR('',#9153,1.);
#2823=VECTOR('',#9154,1.);
#2824=VECTOR('',#9157,1.);
#2825=VECTOR('',#9158,1.);
#2826=VECTOR('',#9159,1.);
#2827=VECTOR('',#9162,1.);
#2828=VECTOR('',#9163,1.);
#2829=VECTOR('',#9164,1.);
#2830=VECTOR('',#9167,1.);
#2831=VECTOR('',#9168,1.);
#2832=VECTOR('',#9169,1.);
#2833=VECTOR('',#9172,1.);
#2834=VECTOR('',#9173,1.);
#2835=VECTOR('',#9174,1.);
#2836=VECTOR('',#9177,1.);
#2837=VECTOR('',#9178,1.);
#2838=VECTOR('',#9179,1.);
#2839=VECTOR('',#9182,1.);
#2840=VECTOR('',#9183,1.);
#2841=VECTOR('',#9184,1.);
#2842=VECTOR('',#9185,1.);
#2843=VECTOR('',#9188,1.);
#2844=VECTOR('',#9189,1.);
#2845=VECTOR('',#9190,1.);
#2846=VECTOR('',#9193,1.);
#2847=VECTOR('',#9194,1.);
#2848=VECTOR('',#9195,1.);
#2849=VECTOR('',#9198,1.);
#2850=VECTOR('',#9199,1.);
#2851=VECTOR('',#9200,1.);
#2852=VECTOR('',#9203,1.);
#2853=VECTOR('',#9204,1.);
#2854=VECTOR('',#9205,1.);
#2855=VECTOR('',#9208,1.);
#2856=VECTOR('',#9209,1.);
#2857=VECTOR('',#9210,1.);
#2858=VECTOR('',#9213,1.);
#2859=VECTOR('',#9214,1.);
#2860=VECTOR('',#9215,1.);
#2861=VECTOR('',#9218,1.);
#2862=VECTOR('',#9219,1.);
#2863=VECTOR('',#9220,1.);
#2864=VECTOR('',#9223,1.);
#2865=VECTOR('',#9224,1.);
#2866=VECTOR('',#9225,1.);
#2867=VECTOR('',#9228,1.);
#2868=VECTOR('',#9229,1.);
#2869=VECTOR('',#9230,1.);
#2870=VECTOR('',#9231,1.);
#2871=VECTOR('',#9234,1.);
#2872=VECTOR('',#9235,1.);
#2873=VECTOR('',#9236,1.);
#2874=VECTOR('',#9239,1.);
#2875=VECTOR('',#9240,1.);
#2876=VECTOR('',#9241,1.);
#2877=VECTOR('',#9244,1.);
#2878=VECTOR('',#9245,1.);
#2879=VECTOR('',#9246,1.);
#2880=VECTOR('',#9249,1.);
#2881=VECTOR('',#9250,1.);
#2882=VECTOR('',#9251,1.);
#2883=VECTOR('',#9254,1.);
#2884=VECTOR('',#9255,1.);
#2885=VECTOR('',#9256,1.);
#2886=VECTOR('',#9259,1.);
#2887=VECTOR('',#9260,1.);
#2888=VECTOR('',#9261,1.);
#2889=VECTOR('',#9264,1.);
#2890=VECTOR('',#9265,1.);
#2891=VECTOR('',#9266,1.);
#2892=VECTOR('',#9269,1.);
#2893=VECTOR('',#9270,1.);
#2894=VECTOR('',#9271,1.);
#2895=VECTOR('',#9274,1.);
#2896=VECTOR('',#9275,1.);
#2897=VECTOR('',#9276,1.);
#2898=VECTOR('',#9277,1.);
#2899=VECTOR('',#9280,1.);
#2900=VECTOR('',#9281,1.);
#2901=VECTOR('',#9282,1.);
#2902=VECTOR('',#9285,1.);
#2903=VECTOR('',#9286,1.);
#2904=VECTOR('',#9287,1.);
#2905=VECTOR('',#9290,1.);
#2906=VECTOR('',#9291,1.);
#2907=VECTOR('',#9292,1.);
#2908=VECTOR('',#9295,1.);
#2909=VECTOR('',#9296,1.);
#2910=VECTOR('',#9297,1.);
#2911=VECTOR('',#9300,1.);
#2912=VECTOR('',#9301,1.);
#2913=VECTOR('',#9302,1.);
#2914=VECTOR('',#9305,1.);
#2915=VECTOR('',#9306,1.);
#2916=VECTOR('',#9307,1.);
#2917=VECTOR('',#9310,1.);
#2918=VECTOR('',#9311,1.);
#2919=VECTOR('',#9312,1.);
#2920=VECTOR('',#9315,1.);
#2921=VECTOR('',#9316,1.);
#2922=VECTOR('',#9317,1.);
#2923=VECTOR('',#9320,0.21);
#2924=VECTOR('',#9325,1.);
#2925=VECTOR('',#9326,1.);
#2926=VECTOR('',#9327,1.);
#2927=VECTOR('',#9330,1.);
#2928=VECTOR('',#9331,1.);
#2929=VECTOR('',#9332,1.);
#2930=VECTOR('',#9335,1.);
#2931=VECTOR('',#9336,1.);
#2932=VECTOR('',#9339,1.);
#2933=VECTOR('',#9340,1.);
#2934=VECTOR('',#9341,1.);
#2935=VECTOR('',#9344,1.);
#2936=VECTOR('',#9345,1.);
#2937=VECTOR('',#9348,1.);
#2938=VECTOR('',#9349,1.);
#2939=VECTOR('',#9350,1.);
#2940=VECTOR('',#9353,1.);
#2941=VECTOR('',#9354,1.);
#2942=VECTOR('',#9357,1.);
#2943=VECTOR('',#9358,1.);
#2944=VECTOR('',#9367,1.);
#2945=VECTOR('',#9368,1.);
#2946=VECTOR('',#9369,1.);
#2947=VECTOR('',#9370,1.);
#2948=VECTOR('',#9373,1.);
#2949=VECTOR('',#9374,1.);
#2950=VECTOR('',#9375,1.);
#2951=VECTOR('',#9378,1.);
#2952=VECTOR('',#9379,1.);
#2953=VECTOR('',#9380,1.);
#2954=VECTOR('',#9383,1.);
#2955=VECTOR('',#9384,1.);
#2956=VECTOR('',#9385,1.);
#2957=VECTOR('',#9388,1.);
#2958=VECTOR('',#9389,1.);
#2959=VECTOR('',#9390,1.);
#2960=VECTOR('',#9393,1.);
#2961=VECTOR('',#9394,1.);
#2962=VECTOR('',#9395,1.);
#2963=VECTOR('',#9398,1.);
#2964=VECTOR('',#9399,1.);
#2965=VECTOR('',#9400,1.);
#2966=VECTOR('',#9403,1.);
#2967=VECTOR('',#9404,1.);
#2968=VECTOR('',#9405,1.);
#2969=VECTOR('',#9408,1.);
#2970=VECTOR('',#9409,1.);
#2971=VECTOR('',#9410,1.);
#2972=VECTOR('',#9413,1.);
#2973=VECTOR('',#9414,1.);
#2974=VECTOR('',#9415,1.);
#2975=VECTOR('',#9416,1.);
#2976=VECTOR('',#9419,1.);
#2977=VECTOR('',#9420,1.);
#2978=VECTOR('',#9421,1.);
#2979=VECTOR('',#9424,1.);
#2980=VECTOR('',#9425,1.);
#2981=VECTOR('',#9426,1.);
#2982=VECTOR('',#9429,1.);
#2983=VECTOR('',#9430,1.);
#2984=VECTOR('',#9431,1.);
#2985=VECTOR('',#9434,1.);
#2986=VECTOR('',#9435,1.);
#2987=VECTOR('',#9436,1.);
#2988=VECTOR('',#9439,1.);
#2989=VECTOR('',#9440,1.);
#2990=VECTOR('',#9441,1.);
#2991=VECTOR('',#9444,1.);
#2992=VECTOR('',#9445,1.);
#2993=VECTOR('',#9446,1.);
#2994=VECTOR('',#9449,1.);
#2995=VECTOR('',#9450,1.);
#2996=VECTOR('',#9451,1.);
#2997=VECTOR('',#9454,1.);
#2998=VECTOR('',#9455,1.);
#2999=VECTOR('',#9456,1.);
#3000=VECTOR('',#9459,1.);
#3001=VECTOR('',#9460,1.);
#3002=VECTOR('',#9461,1.);
#3003=VECTOR('',#9462,1.);
#3004=VECTOR('',#9465,1.);
#3005=VECTOR('',#9466,1.);
#3006=VECTOR('',#9467,1.);
#3007=VECTOR('',#9470,1.);
#3008=VECTOR('',#9471,1.);
#3009=VECTOR('',#9472,1.);
#3010=VECTOR('',#9475,1.);
#3011=VECTOR('',#9476,1.);
#3012=VECTOR('',#9477,1.);
#3013=VECTOR('',#9480,1.);
#3014=VECTOR('',#9481,1.);
#3015=VECTOR('',#9482,1.);
#3016=VECTOR('',#9485,1.);
#3017=VECTOR('',#9486,1.);
#3018=VECTOR('',#9487,1.);
#3019=VECTOR('',#9490,1.);
#3020=VECTOR('',#9491,1.);
#3021=VECTOR('',#9492,1.);
#3022=VECTOR('',#9495,1.);
#3023=VECTOR('',#9496,1.);
#3024=VECTOR('',#9497,1.);
#3025=VECTOR('',#9500,1.);
#3026=VECTOR('',#9501,1.);
#3027=VECTOR('',#9502,1.);
#3028=VECTOR('',#9505,1.);
#3029=VECTOR('',#9506,1.);
#3030=VECTOR('',#9507,1.);
#3031=VECTOR('',#9508,1.);
#3032=VECTOR('',#9511,1.);
#3033=VECTOR('',#9512,1.);
#3034=VECTOR('',#9513,1.);
#3035=VECTOR('',#9516,1.);
#3036=VECTOR('',#9517,1.);
#3037=VECTOR('',#9518,1.);
#3038=VECTOR('',#9521,1.);
#3039=VECTOR('',#9522,1.);
#3040=VECTOR('',#9523,1.);
#3041=VECTOR('',#9526,1.);
#3042=VECTOR('',#9527,1.);
#3043=VECTOR('',#9528,1.);
#3044=VECTOR('',#9531,1.);
#3045=VECTOR('',#9532,1.);
#3046=VECTOR('',#9533,1.);
#3047=VECTOR('',#9536,1.);
#3048=VECTOR('',#9537,1.);
#3049=VECTOR('',#9538,1.);
#3050=VECTOR('',#9541,1.);
#3051=VECTOR('',#9542,1.);
#3052=VECTOR('',#9543,1.);
#3053=VECTOR('',#9546,1.);
#3054=VECTOR('',#9547,1.);
#3055=VECTOR('',#9548,1.);
#3056=VECTOR('',#9553,0.21);
#3057=VECTOR('',#9558,1.);
#3058=VECTOR('',#9559,1.);
#3059=VECTOR('',#9560,1.);
#3060=VECTOR('',#9563,1.);
#3061=VECTOR('',#9564,1.);
#3062=VECTOR('',#9565,1.);
#3063=VECTOR('',#9568,1.);
#3064=VECTOR('',#9569,1.);
#3065=VECTOR('',#9572,1.);
#3066=VECTOR('',#9573,1.);
#3067=VECTOR('',#9574,1.);
#3068=VECTOR('',#9577,1.);
#3069=VECTOR('',#9578,1.);
#3070=VECTOR('',#9581,1.);
#3071=VECTOR('',#9582,1.);
#3072=VECTOR('',#9583,1.);
#3073=VECTOR('',#9586,1.);
#3074=VECTOR('',#9587,1.);
#3075=VECTOR('',#9590,1.);
#3076=VECTOR('',#9591,1.);
#3077=VECTOR('',#9600,1.);
#3078=VECTOR('',#9601,1.);
#3079=VECTOR('',#9602,1.);
#3080=VECTOR('',#9603,1.);
#3081=VECTOR('',#9606,1.);
#3082=VECTOR('',#9607,1.);
#3083=VECTOR('',#9608,1.);
#3084=VECTOR('',#9611,1.);
#3085=VECTOR('',#9612,1.);
#3086=VECTOR('',#9613,1.);
#3087=VECTOR('',#9616,1.);
#3088=VECTOR('',#9617,1.);
#3089=VECTOR('',#9618,1.);
#3090=VECTOR('',#9621,1.);
#3091=VECTOR('',#9622,1.);
#3092=VECTOR('',#9623,1.);
#3093=VECTOR('',#9626,1.);
#3094=VECTOR('',#9627,1.);
#3095=VECTOR('',#9640,0.25);
#3096=VECTOR('',#9653,0.4);
#3097=VECTOR('',#9658,0.425);
#3098=VECTOR('',#9663,0.41);
#3099=VECTOR('',#9672,0.26);
#3100=VECTOR('',#9675,0.25);
#3101=VECTOR('',#9686,0.4);
#3102=VECTOR('',#9691,0.425);
#3103=VECTOR('',#9696,0.41);
#3104=VECTOR('',#9705,0.26);
#3105=VECTOR('',#9710,0.25);
#3106=VECTOR('',#9715,0.225);
#3107=VECTOR('',#9720,1.);
#3108=VECTOR('',#9721,1.);
#3109=VECTOR('',#9722,1.);
#3110=VECTOR('',#9723,1.);
#3111=VECTOR('',#9726,1.);
#3112=VECTOR('',#9727,1.);
#3113=VECTOR('',#9728,1.);
#3114=VECTOR('',#9731,1.);
#3115=VECTOR('',#9732,1.);
#3116=VECTOR('',#9733,1.);
#3117=VECTOR('',#9736,1.);
#3118=VECTOR('',#9737,1.);
#3119=VECTOR('',#9738,1.);
#3120=VECTOR('',#9741,1.);
#3121=VECTOR('',#9742,1.);
#3122=VECTOR('',#9743,1.);
#3123=VECTOR('',#9746,1.);
#3124=VECTOR('',#9747,1.);
#3125=VECTOR('',#9758,0.274999999999999);
#3126=VECTOR('',#9765,0.274999999999999);
#3127=VECTOR('',#9772,0.274999999999999);
#3128=VECTOR('',#9779,0.274999999999999);
#3129=VECTOR('',#9784,1.);
#3130=VECTOR('',#9785,1.);
#3131=VECTOR('',#9786,1.);
#3132=VECTOR('',#9787,1.);
#3133=VECTOR('',#9790,1.);
#3134=VECTOR('',#9791,1.);
#3135=VECTOR('',#9792,1.);
#3136=VECTOR('',#9795,1.);
#3137=VECTOR('',#9796,1.);
#3138=VECTOR('',#9797,1.);
#3139=VECTOR('',#9800,1.);
#3140=VECTOR('',#9801,1.);
#3141=VECTOR('',#9812,0.275);
#3142=VECTOR('',#9817,0.265);
#3143=VECTOR('',#9826,0.5);
#3144=VECTOR('',#9837,0.275);
#3145=VECTOR('',#9844,0.275);
#3146=VECTOR('',#9849,1.);
#3147=VECTOR('',#9850,1.);
#3148=VECTOR('',#9851,1.);
#3149=VECTOR('',#9852,1.);
#3150=VECTOR('',#9855,1.);
#3151=VECTOR('',#9856,1.);
#3152=VECTOR('',#9857,1.);
#3153=VECTOR('',#9860,1.);
#3154=VECTOR('',#9861,1.);
#3155=VECTOR('',#9862,1.);
#3156=VECTOR('',#9865,1.);
#3157=VECTOR('',#9866,1.);
#3158=VECTOR('',#9875,1.);
#3159=VECTOR('',#9876,1.);
#3160=VECTOR('',#9877,1.);
#3161=VECTOR('',#9878,1.);
#3162=VECTOR('',#9881,1.);
#3163=VECTOR('',#9882,1.);
#3164=VECTOR('',#9883,1.);
#3165=VECTOR('',#9886,1.);
#3166=VECTOR('',#9887,1.);
#3167=VECTOR('',#9888,1.);
#3168=VECTOR('',#9891,1.);
#3169=VECTOR('',#9892,1.);
#3170=VECTOR('',#9901,1.);
#3171=VECTOR('',#9902,1.);
#3172=VECTOR('',#9903,1.);
#3173=VECTOR('',#9904,1.);
#3174=VECTOR('',#9907,1.);
#3175=VECTOR('',#9908,1.);
#3176=VECTOR('',#9909,1.);
#3177=VECTOR('',#9912,1.);
#3178=VECTOR('',#9913,1.);
#3179=VECTOR('',#9914,1.);
#3180=VECTOR('',#9917,1.);
#3181=VECTOR('',#9918,1.);
#3182=VECTOR('',#9929,0.274999999999999);
#3183=VECTOR('',#9936,0.274999999999999);
#3184=VECTOR('',#9941,1.);
#3185=VECTOR('',#9942,1.);
#3186=VECTOR('',#9943,1.);
#3187=VECTOR('',#9944,1.);
#3188=VECTOR('',#9947,1.);
#3189=VECTOR('',#9948,1.);
#3190=VECTOR('',#9949,1.);
#3191=VECTOR('',#9952,1.);
#3192=VECTOR('',#9953,1.);
#3193=VECTOR('',#9954,1.);
#3194=VECTOR('',#9957,1.);
#3195=VECTOR('',#9958,1.);
#3196=VECTOR('',#9967,1.);
#3197=VECTOR('',#9968,1.);
#3198=VECTOR('',#9969,1.);
#3199=VECTOR('',#9970,1.);
#3200=VECTOR('',#9973,1.);
#3201=VECTOR('',#9974,1.);
#3202=VECTOR('',#9975,1.);
#3203=VECTOR('',#9978,1.);
#3204=VECTOR('',#9979,1.);
#3205=VECTOR('',#9980,1.);
#3206=VECTOR('',#9983,1.);
#3207=VECTOR('',#9984,1.);
#3208=VECTOR('',#9993,1.);
#3209=VECTOR('',#9994,1.);
#3210=VECTOR('',#9995,1.);
#3211=VECTOR('',#9996,1.);
#3212=VECTOR('',#9999,1.);
#3213=VECTOR('',#10000,1.);
#3214=VECTOR('',#10001,1.);
#3215=VECTOR('',#10004,1.);
#3216=VECTOR('',#10005,1.);
#3217=VECTOR('',#10006,1.);
#3218=VECTOR('',#10009,1.);
#3219=VECTOR('',#10010,1.);
#3220=VECTOR('',#10023,1.7);
#3221=VECTOR('',#10030,2.);
#3222=VECTOR('',#10043,1.1);
#3223=VECTOR('',#10052,1.5);
#3224=VECTOR('',#10059,1.7);
#3225=VECTOR('',#10072,1.5);
#3226=VECTOR('',#10081,1.2);
#3227=VECTOR('',#10088,2.);
#3228=VECTOR('',#10101,1.1);
#3229=VECTOR('',#10112,1.5);
#3230=VECTOR('',#10117,1.7);
#3231=VECTOR('',#10130,1.5);
#3232=VECTOR('',#10141,1.2);
#3233=VECTOR('',#10146,2.);
#3234=VECTOR('',#10159,0.165);
#3235=VECTOR('',#10168,0.165);
#3236=VECTOR('',#10177,0.5);
#3237=VECTOR('',#10190,0.5);
#3238=VECTOR('',#10201,0.5);
#3239=VECTOR('',#10212,0.275);
#3240=VECTOR('',#10217,0.275);
#3241=VECTOR('',#10222,0.505);
#3242=VECTOR('',#10227,1.);
#3243=VECTOR('',#10228,1.);
#3244=VECTOR('',#10229,1.);
#3245=VECTOR('',#10230,1.);
#3246=VECTOR('',#10233,1.);
#3247=VECTOR('',#10234,1.);
#3248=VECTOR('',#10235,1.);
#3249=VECTOR('',#10238,1.);
#3250=VECTOR('',#10239,1.);
#3251=VECTOR('',#10240,1.);
#3252=VECTOR('',#10243,1.);
#3253=VECTOR('',#10244,1.);
#3254=VECTOR('',#10255,0.225);
#3255=VECTOR('',#10262,0.7);
#3256=VECTOR('',#10275,0.505);
#3257=VECTOR('',#10282,0.7);
#3258=VECTOR('',#10307,0.976185);
#3259=VECTOR('',#10314,0.5);
#3260=VECTOR('',#10319,0.53);
#3261=VECTOR('',#10328,0.976185);
#3262=VECTOR('',#10335,0.53);
#3263=VECTOR('',#10354,1.023815);
#3264=VECTOR('',#10365,1.47);
#3265=VECTOR('',#10370,1.5);
#3266=VECTOR('',#10375,1.47);
#3267=VECTOR('',#10380,1.023815);
#3268=VECTOR('',#10431,1.019052);
#3269=VECTOR('',#10508,0.980948);
#3270=VECTOR('',#10537,1.013815);
#3271=VECTOR('',#10544,0.991185);
#3272=VECTOR('',#10555,1.013815);
#3273=VECTOR('',#10562,0.991185);
#3274=VECTOR('',#10579,0.505);
#3275=VECTOR('',#10586,0.7);
#3276=VECTOR('',#10597,1.);
#3277=VECTOR('',#10598,1.);
#3278=VECTOR('',#10599,1.);
#3279=VECTOR('',#10600,1.);
#3280=VECTOR('',#10603,1.);
#3281=VECTOR('',#10604,1.);
#3282=VECTOR('',#10605,1.);
#3283=VECTOR('',#10608,1.);
#3284=VECTOR('',#10609,1.);
#3285=VECTOR('',#10610,1.);
#3286=VECTOR('',#10613,1.);
#3287=VECTOR('',#10614,1.);
#3288=VECTOR('',#10615,1.);
#3289=VECTOR('',#10618,1.);
#3290=VECTOR('',#10619,1.);
#3291=VECTOR('',#10620,1.);
#3292=VECTOR('',#10623,1.);
#3293=VECTOR('',#10624,1.);
#3294=VECTOR('',#10641,0.325);
#3295=VECTOR('',#10646,0.35);
#3296=VECTOR('',#10651,0.335);
#3297=VECTOR('',#10660,0.21);
#3298=VECTOR('',#10663,0.2);
#3299=VECTOR('',#10670,0.225);
#3300=VECTOR('',#10677,0.7);
#3301=VECTOR('',#10688,1.);
#3302=VECTOR('',#10689,1.);
#3303=VECTOR('',#10690,1.);
#3304=VECTOR('',#10691,1.);
#3305=VECTOR('',#10694,1.);
#3306=VECTOR('',#10695,1.);
#3307=VECTOR('',#10696,1.);
#3308=VECTOR('',#10699,1.);
#3309=VECTOR('',#10700,1.);
#3310=VECTOR('',#10701,1.);
#3311=VECTOR('',#10706,1.);
#3312=VECTOR('',#10707,1.);
#3313=VECTOR('',#10708,1.);
#3314=VECTOR('',#10709,1.);
#3315=VECTOR('',#10710,1.);
#3316=VECTOR('',#10711,1.);
#3317=VECTOR('',#10712,1.);
#3318=VECTOR('',#10715,1.);
#3319=VECTOR('',#10716,1.);
#3320=VECTOR('',#10719,1.);
#3321=VECTOR('',#10720,1.);
#3322=VECTOR('',#10723,1.);
#3323=VECTOR('',#10724,1.);
#3324=VECTOR('',#10725,1.);
#3325=VECTOR('',#10726,1.);
#3326=VECTOR('',#10727,1.);
#3327=VECTOR('',#10730,1.);
#3328=VECTOR('',#10733,1.);
#3329=VECTOR('',#10736,1.);
#3330=VECTOR('',#10741,0.21);
#3331=VECTOR('',#10750,1.);
#3332=VECTOR('',#10753,1.);
#3333=VECTOR('',#10756,1.);
#3334=VECTOR('',#10763,1.);
#3335=VECTOR('',#10764,1.);
#3336=VECTOR('',#10765,1.);
#3337=VECTOR('',#10766,1.);
#3338=VECTOR('',#10769,1.);
#3339=VECTOR('',#10770,1.);
#3340=VECTOR('',#10771,1.);
#3341=VECTOR('',#10774,1.);
#3342=VECTOR('',#10775,1.);
#3343=VECTOR('',#10776,1.);
#3344=VECTOR('',#10779,1.);
#3345=VECTOR('',#10780,1.);
#3346=VECTOR('',#10781,1.);
#3347=VECTOR('',#10784,1.);
#3348=VECTOR('',#10785,1.);
#3349=VECTOR('',#10786,1.);
#3350=VECTOR('',#10789,1.);
#3351=VECTOR('',#10790,1.);
#3352=VECTOR('',#10807,0.4);
#3353=VECTOR('',#10812,0.425);
#3354=VECTOR('',#10817,0.41);
#3355=VECTOR('',#10826,0.26);
#3356=VECTOR('',#10829,0.25);
#3357=VECTOR('',#10948,0.5);
#3358=VECTOR('',#10959,0.5);
#3359=VECTOR('',#10970,0.275);
#3360=VECTOR('',#10975,0.275);
#3361=VECTOR('',#10980,0.505);
#3362=VECTOR('',#10985,1.);
#3363=VECTOR('',#10986,1.);
#3364=VECTOR('',#10987,1.);
#3365=VECTOR('',#10988,1.);
#3366=VECTOR('',#10991,1.);
#3367=VECTOR('',#10992,1.);
#3368=VECTOR('',#10993,1.);
#3369=VECTOR('',#10996,1.);
#3370=VECTOR('',#10997,1.);
#3371=VECTOR('',#10998,1.);
#3372=VECTOR('',#11001,1.);
#3373=VECTOR('',#11002,1.);
#3374=CIRCLE('',#8052,0.274999999999999);
#3375=CIRCLE('',#8053,0.274999999999999);
#3376=CIRCLE('',#8055,0.274999999999999);
#3377=CIRCLE('',#8056,0.274999999999999);
#3378=CIRCLE('',#8058,0.274999999999999);
#3379=CIRCLE('',#8059,0.274999999999999);
#3380=CIRCLE('',#8061,0.274999999999999);
#3381=CIRCLE('',#8062,0.274999999999999);
#3382=CIRCLE('',#8071,0.275);
#3383=CIRCLE('',#8072,0.275);
#3384=CIRCLE('',#8074,0.21);
#3385=CIRCLE('',#8112,0.21);
#3386=CIRCLE('',#8125,0.275);
#3387=CIRCLE('',#8126,0.275);
#3388=CIRCLE('',#8128,0.21);
#3389=CIRCLE('',#8166,0.21);
#3390=CIRCLE('',#8215,0.21);
#3391=CIRCLE('',#8216,0.21);
#3392=CIRCLE('',#8237,0.25);
#3393=CIRCLE('',#8238,0.24505);
#3394=CIRCLE('',#8240,0.25);
#3395=CIRCLE('',#8243,0.375);
#3396=CIRCLE('',#8245,0.425);
#3397=CIRCLE('',#8247,0.425);
#3398=CIRCLE('',#8249,0.395);
#3399=CIRCLE('',#8251,0.27);
#3400=CIRCLE('',#8253,0.24505);
#3401=CIRCLE('',#8257,0.375);
#3402=CIRCLE('',#8259,0.425);
#3403=CIRCLE('',#8261,0.425);
#3404=CIRCLE('',#8263,0.395);
#3405=CIRCLE('',#8265,0.27);
#3406=CIRCLE('',#8267,0.24505);
#3407=CIRCLE('',#8269,0.24505);
#3408=CIRCLE('',#8271,0.2);
#3409=CIRCLE('',#8283,0.274999999999999);
#3410=CIRCLE('',#8284,0.274999999999999);
#3411=CIRCLE('',#8286,0.274999999999999);
#3412=CIRCLE('',#8287,0.274999999999999);
#3413=CIRCLE('',#8289,0.274999999999999);
#3414=CIRCLE('',#8290,0.274999999999999);
#3415=CIRCLE('',#8292,0.274999999999999);
#3416=CIRCLE('',#8293,0.274999999999999);
#3417=CIRCLE('',#8302,0.285);
#3418=CIRCLE('',#8303,0.265);
#3419=CIRCLE('',#8305,0.265);
#3420=CIRCLE('',#8307,0.5);
#3421=CIRCLE('',#8309,0.5);
#3422=CIRCLE('',#8313,0.275);
#3423=CIRCLE('',#8314,0.275);
#3424=CIRCLE('',#8316,0.275);
#3425=CIRCLE('',#8317,0.275);
#3426=CIRCLE('',#8340,0.274999999999999);
#3427=CIRCLE('',#8341,0.274999999999999);
#3428=CIRCLE('',#8343,0.274999999999999);
#3429=CIRCLE('',#8344,0.274999999999999);
#3430=CIRCLE('',#8368,1.7);
#3431=CIRCLE('',#8369,1.7);
#3432=CIRCLE('',#8371,2.);
#3433=CIRCLE('',#8372,2.);
#3434=CIRCLE('',#8377,1.1);
#3435=CIRCLE('',#8378,1.1);
#3436=CIRCLE('',#8380,1.5);
#3437=CIRCLE('',#8382,1.5);
#3438=CIRCLE('',#8384,1.7);
#3439=CIRCLE('',#8385,1.7);
#3440=CIRCLE('',#8390,1.5);
#3441=CIRCLE('',#8391,1.5);
#3442=CIRCLE('',#8393,1.2);
#3443=CIRCLE('',#8395,1.2);
#3444=CIRCLE('',#8397,2.);
#3445=CIRCLE('',#8398,2.);
#3446=CIRCLE('',#8403,1.1);
#3447=CIRCLE('',#8404,1.1);
#3448=CIRCLE('',#8406,1.5);
#3449=CIRCLE('',#8408,1.5);
#3450=CIRCLE('',#8410,1.7);
#3451=CIRCLE('',#8411,1.7);
#3452=CIRCLE('',#8416,1.5);
#3453=CIRCLE('',#8417,1.5);
#3454=CIRCLE('',#8419,1.2);
#3455=CIRCLE('',#8421,1.2);
#3456=CIRCLE('',#8423,2.);
#3457=CIRCLE('',#8424,2.);
#3458=CIRCLE('',#8429,0.165);
#3459=CIRCLE('',#8430,0.165);
#3460=CIRCLE('',#8433,0.165);
#3461=CIRCLE('',#8434,0.165);
#3462=CIRCLE('',#8437,0.5);
#3463=CIRCLE('',#8438,0.5);
#3464=CIRCLE('',#8443,0.5);
#3465=CIRCLE('',#8444,0.5);
#3466=CIRCLE('',#8446,0.275);
#3467=CIRCLE('',#8448,0.5);
#3468=CIRCLE('',#8449,0.5);
#3469=CIRCLE('',#8451,0.275);
#3470=CIRCLE('',#8453,0.275);
#3471=CIRCLE('',#8455,0.275);
#3472=CIRCLE('',#8457,0.505);
#3473=CIRCLE('',#8458,0.505);
#3474=CIRCLE('',#8467,0.225);
#3475=CIRCLE('',#8468,0.225);
#3476=CIRCLE('',#8470,0.7);
#3477=CIRCLE('',#8471,0.7);
#3478=CIRCLE('',#8476,0.505);
#3479=CIRCLE('',#8477,0.505);
#3480=CIRCLE('',#8479,0.7);
#3481=CIRCLE('',#8480,0.7);
#3482=CIRCLE('',#8486,0.976185);
#3483=CIRCLE('',#8487,0.976185);
#3484=CIRCLE('',#8488,0.247676);
#3485=CIRCLE('',#8489,0.976185);
#3486=CIRCLE('',#8490,0.976185);
#3487=CIRCLE('',#8492,0.976185);
#3488=CIRCLE('',#8494,0.5);
#3489=CIRCLE('',#8495,0.5);
#3490=CIRCLE('',#8497,0.56);
#3491=CIRCLE('',#8500,0.976185);
#3492=CIRCLE('',#8502,0.56);
#3493=CIRCLE('',#8506,1.023815);
#3494=CIRCLE('',#8507,1.023815);
#3495=CIRCLE('',#8508,0.247676);
#3496=CIRCLE('',#8509,1.023815);
#3497=CIRCLE('',#8510,1.023815);
#3498=CIRCLE('',#8512,1.023815);
#3499=CIRCLE('',#8514,1.44);
#3500=CIRCLE('',#8515,1.023815);
#3501=CIRCLE('',#8517,1.5);
#3502=CIRCLE('',#8519,1.5);
#3503=CIRCLE('',#8521,1.44);
#3504=CIRCLE('',#8526,0.23815);
#3505=CIRCLE('',#8528,0.23815);
#3506=CIRCLE('',#8530,0.23815);
#3507=CIRCLE('',#8532,0.23815);
#3508=CIRCLE('',#8534,0.23815);
#3509=CIRCLE('',#8536,0.23815);
#3510=CIRCLE('',#8538,0.23815);
#3511=CIRCLE('',#8540,0.23815);
#3512=CIRCLE('',#8543,0.243053047864041);
#3513=CIRCLE('',#8544,0.243053047864041);
#3514=CIRCLE('',#8546,1.019052);
#3515=CIRCLE('',#8547,1.019052);
#3516=CIRCLE('',#8548,1.019052);
#3517=CIRCLE('',#8549,1.019052);
#3518=CIRCLE('',#8550,1.019052);
#3519=CIRCLE('',#8551,1.019052);
#3520=CIRCLE('',#8552,1.019052);
#3521=CIRCLE('',#8553,1.019052);
#3522=CIRCLE('',#8554,1.019052);
#3523=CIRCLE('',#8556,0.980948);
#3524=CIRCLE('',#8557,0.243053047864041);
#3525=CIRCLE('',#8559,0.243053047864041);
#3526=CIRCLE('',#8561,0.980948);
#3527=CIRCLE('',#8562,0.243053047864041);
#3528=CIRCLE('',#8564,0.243053047864041);
#3529=CIRCLE('',#8566,0.980948);
#3530=CIRCLE('',#8567,0.243053047864041);
#3531=CIRCLE('',#8569,0.243053047864041);
#3532=CIRCLE('',#8571,0.980948);
#3533=CIRCLE('',#8572,0.243053047864041);
#3534=CIRCLE('',#8574,0.243053047864041);
#3535=CIRCLE('',#8576,0.980948);
#3536=CIRCLE('',#8577,0.243053047864041);
#3537=CIRCLE('',#8579,0.243053047864041);
#3538=CIRCLE('',#8581,0.980948);
#3539=CIRCLE('',#8582,0.243053047864041);
#3540=CIRCLE('',#8584,0.243053047864041);
#3541=CIRCLE('',#8586,0.980948);
#3542=CIRCLE('',#8587,0.980948);
#3543=CIRCLE('',#8588,0.980948);
#3544=CIRCLE('',#8590,0.243053047864041);
#3545=CIRCLE('',#8592,0.243053047864041);
#3546=CIRCLE('',#8597,1.013815);
#3547=CIRCLE('',#8598,0.991185);
#3548=CIRCLE('',#8600,1.013815);
#3549=CIRCLE('',#8602,0.991185);
#3550=CIRCLE('',#8605,1.013815);
#3551=CIRCLE('',#8606,0.991185);
#3552=CIRCLE('',#8608,1.013815);
#3553=CIRCLE('',#8610,0.991185);
#3554=CIRCLE('',#8619,0.505);
#3555=CIRCLE('',#8620,0.505);
#3556=CIRCLE('',#8622,0.7);
#3557=CIRCLE('',#8623,0.7);
#3558=CIRCLE('',#8636,0.1954);
#3559=CIRCLE('',#8638,0.3);
#3560=CIRCLE('',#8640,0.35);
#3561=CIRCLE('',#8642,0.35);
#3562=CIRCLE('',#8644,0.32);
#3563=CIRCLE('',#8646,0.22);
#3564=CIRCLE('',#8648,0.1954);
#3565=CIRCLE('',#8652,0.225);
#3566=CIRCLE('',#8653,0.225);
#3567=CIRCLE('',#8655,0.7);
#3568=CIRCLE('',#8656,0.7);
#3569=CIRCLE('',#8663,0.2117);
#3570=CIRCLE('',#8672,0.2117);
#3571=CIRCLE('',#8673,0.2117);
#3572=CIRCLE('',#8675,0.2117);
#3573=CIRCLE('',#8690,0.24505);
#3574=CIRCLE('',#8692,0.375);
#3575=CIRCLE('',#8694,0.425);
#3576=CIRCLE('',#8696,0.425);
#3577=CIRCLE('',#8698,0.395);
#3578=CIRCLE('',#8700,0.27);
#3579=CIRCLE('',#8702,0.24505);
#3580=CIRCLE('',#8762,0.5);
#3581=CIRCLE('',#8763,0.5);
#3582=CIRCLE('',#8765,0.275);
#3583=CIRCLE('',#8767,0.5);
#3584=CIRCLE('',#8768,0.5);
#3585=CIRCLE('',#8770,0.275);
#3586=CIRCLE('',#8772,0.275);
#3587=CIRCLE('',#8774,0.275);
#3588=CIRCLE('',#8776,0.505);
#3589=CIRCLE('',#8777,0.505);
#3590=VERTEX_POINT('',#11077);
#3591=VERTEX_POINT('',#11079);
#3592=VERTEX_POINT('',#11083);
#3593=VERTEX_POINT('',#11085);
#3594=VERTEX_POINT('',#11089);
#3595=VERTEX_POINT('',#11091);
#3596=VERTEX_POINT('',#11095);
#3597=VERTEX_POINT('',#11097);
#3598=VERTEX_POINT('',#11101);
#3599=VERTEX_POINT('',#11102);
#3600=VERTEX_POINT('',#11104);
#3601=VERTEX_POINT('',#11106);
#3602=VERTEX_POINT('',#11110);
#3603=VERTEX_POINT('',#11112);
#3604=VERTEX_POINT('',#11116);
#3605=VERTEX_POINT('',#11118);
#3606=VERTEX_POINT('',#11128);
#3607=VERTEX_POINT('',#11130);
#3608=VERTEX_POINT('',#11132);
#3609=VERTEX_POINT('',#11155);
#3610=VERTEX_POINT('',#11158);
#3611=VERTEX_POINT('',#11183);
#3612=VERTEX_POINT('',#11184);
#3613=VERTEX_POINT('',#11230);
#3614=VERTEX_POINT('',#11234);
#3615=VERTEX_POINT('',#11235);
#3616=VERTEX_POINT('',#11237);
#3617=VERTEX_POINT('',#11239);
#3618=VERTEX_POINT('',#11243);
#3619=VERTEX_POINT('',#11245);
#3620=VERTEX_POINT('',#11249);
#3621=VERTEX_POINT('',#11251);
#3622=VERTEX_POINT('',#11255);
#3623=VERTEX_POINT('',#11257);
#3624=VERTEX_POINT('',#11261);
#3625=VERTEX_POINT('',#11263);
#3626=VERTEX_POINT('',#11267);
#3627=VERTEX_POINT('',#11269);
#3628=VERTEX_POINT('',#11273);
#3629=VERTEX_POINT('',#11275);
#3630=VERTEX_POINT('',#11279);
#3631=VERTEX_POINT('',#11281);
#3632=VERTEX_POINT('',#11285);
#3633=VERTEX_POINT('',#11287);
#3634=VERTEX_POINT('',#11291);
#3635=VERTEX_POINT('',#11292);
#3636=VERTEX_POINT('',#11294);
#3637=VERTEX_POINT('',#11296);
#3638=VERTEX_POINT('',#11300);
#3639=VERTEX_POINT('',#11302);
#3640=VERTEX_POINT('',#11306);
#3641=VERTEX_POINT('',#11308);
#3642=VERTEX_POINT('',#11312);
#3643=VERTEX_POINT('',#11314);
#3644=VERTEX_POINT('',#11318);
#3645=VERTEX_POINT('',#11320);
#3646=VERTEX_POINT('',#11324);
#3647=VERTEX_POINT('',#11326);
#3648=VERTEX_POINT('',#11330);
#3649=VERTEX_POINT('',#11332);
#3650=VERTEX_POINT('',#11336);
#3651=VERTEX_POINT('',#11338);
#3652=VERTEX_POINT('',#11342);
#3653=VERTEX_POINT('',#11344);
#3654=VERTEX_POINT('',#11348);
#3655=VERTEX_POINT('',#11349);
#3656=VERTEX_POINT('',#11351);
#3657=VERTEX_POINT('',#11353);
#3658=VERTEX_POINT('',#11357);
#3659=VERTEX_POINT('',#11359);
#3660=VERTEX_POINT('',#11363);
#3661=VERTEX_POINT('',#11365);
#3662=VERTEX_POINT('',#11369);
#3663=VERTEX_POINT('',#11371);
#3664=VERTEX_POINT('',#11375);
#3665=VERTEX_POINT('',#11377);
#3666=VERTEX_POINT('',#11381);
#3667=VERTEX_POINT('',#11383);
#3668=VERTEX_POINT('',#11387);
#3669=VERTEX_POINT('',#11389);
#3670=VERTEX_POINT('',#11393);
#3671=VERTEX_POINT('',#11395);
#3672=VERTEX_POINT('',#11399);
#3673=VERTEX_POINT('',#11401);
#3674=VERTEX_POINT('',#11405);
#3675=VERTEX_POINT('',#11406);
#3676=VERTEX_POINT('',#11408);
#3677=VERTEX_POINT('',#11410);
#3678=VERTEX_POINT('',#11414);
#3679=VERTEX_POINT('',#11416);
#3680=VERTEX_POINT('',#11420);
#3681=VERTEX_POINT('',#11422);
#3682=VERTEX_POINT('',#11426);
#3683=VERTEX_POINT('',#11428);
#3684=VERTEX_POINT('',#11432);
#3685=VERTEX_POINT('',#11434);
#3686=VERTEX_POINT('',#11438);
#3687=VERTEX_POINT('',#11440);
#3688=VERTEX_POINT('',#11444);
#3689=VERTEX_POINT('',#11446);
#3690=VERTEX_POINT('',#11450);
#3691=VERTEX_POINT('',#11452);
#3692=VERTEX_POINT('',#11456);
#3693=VERTEX_POINT('',#11458);
#3694=VERTEX_POINT('',#11462);
#3695=VERTEX_POINT('',#11466);
#3696=VERTEX_POINT('',#11468);
#3697=VERTEX_POINT('',#11472);
#3698=VERTEX_POINT('',#11474);
#3699=VERTEX_POINT('',#11481);
#3700=VERTEX_POINT('',#11483);
#3701=VERTEX_POINT('',#11490);
#3702=VERTEX_POINT('',#11492);
#3703=VERTEX_POINT('',#11505);
#3704=VERTEX_POINT('',#11507);
#3705=VERTEX_POINT('',#11509);
#3706=VERTEX_POINT('',#11532);
#3707=VERTEX_POINT('',#11535);
#3708=VERTEX_POINT('',#11560);
#3709=VERTEX_POINT('',#11561);
#3710=VERTEX_POINT('',#11607);
#3711=VERTEX_POINT('',#11611);
#3712=VERTEX_POINT('',#11612);
#3713=VERTEX_POINT('',#11614);
#3714=VERTEX_POINT('',#11616);
#3715=VERTEX_POINT('',#11620);
#3716=VERTEX_POINT('',#11622);
#3717=VERTEX_POINT('',#11626);
#3718=VERTEX_POINT('',#11628);
#3719=VERTEX_POINT('',#11632);
#3720=VERTEX_POINT('',#11634);
#3721=VERTEX_POINT('',#11638);
#3722=VERTEX_POINT('',#11640);
#3723=VERTEX_POINT('',#11644);
#3724=VERTEX_POINT('',#11646);
#3725=VERTEX_POINT('',#11650);
#3726=VERTEX_POINT('',#11652);
#3727=VERTEX_POINT('',#11656);
#3728=VERTEX_POINT('',#11658);
#3729=VERTEX_POINT('',#11662);
#3730=VERTEX_POINT('',#11664);
#3731=VERTEX_POINT('',#11668);
#3732=VERTEX_POINT('',#11669);
#3733=VERTEX_POINT('',#11671);
#3734=VERTEX_POINT('',#11673);
#3735=VERTEX_POINT('',#11677);
#3736=VERTEX_POINT('',#11679);
#3737=VERTEX_POINT('',#11683);
#3738=VERTEX_POINT('',#11685);
#3739=VERTEX_POINT('',#11689);
#3740=VERTEX_POINT('',#11691);
#3741=VERTEX_POINT('',#11695);
#3742=VERTEX_POINT('',#11697);
#3743=VERTEX_POINT('',#11701);
#3744=VERTEX_POINT('',#11703);
#3745=VERTEX_POINT('',#11707);
#3746=VERTEX_POINT('',#11709);
#3747=VERTEX_POINT('',#11713);
#3748=VERTEX_POINT('',#11715);
#3749=VERTEX_POINT('',#11719);
#3750=VERTEX_POINT('',#11721);
#3751=VERTEX_POINT('',#11725);
#3752=VERTEX_POINT('',#11726);
#3753=VERTEX_POINT('',#11728);
#3754=VERTEX_POINT('',#11730);
#3755=VERTEX_POINT('',#11734);
#3756=VERTEX_POINT('',#11736);
#3757=VERTEX_POINT('',#11740);
#3758=VERTEX_POINT('',#11742);
#3759=VERTEX_POINT('',#11746);
#3760=VERTEX_POINT('',#11748);
#3761=VERTEX_POINT('',#11752);
#3762=VERTEX_POINT('',#11754);
#3763=VERTEX_POINT('',#11758);
#3764=VERTEX_POINT('',#11760);
#3765=VERTEX_POINT('',#11764);
#3766=VERTEX_POINT('',#11766);
#3767=VERTEX_POINT('',#11770);
#3768=VERTEX_POINT('',#11772);
#3769=VERTEX_POINT('',#11776);
#3770=VERTEX_POINT('',#11778);
#3771=VERTEX_POINT('',#11782);
#3772=VERTEX_POINT('',#11783);
#3773=VERTEX_POINT('',#11785);
#3774=VERTEX_POINT('',#11787);
#3775=VERTEX_POINT('',#11791);
#3776=VERTEX_POINT('',#11793);
#3777=VERTEX_POINT('',#11797);
#3778=VERTEX_POINT('',#11799);
#3779=VERTEX_POINT('',#11803);
#3780=VERTEX_POINT('',#11805);
#3781=VERTEX_POINT('',#11809);
#3782=VERTEX_POINT('',#11811);
#3783=VERTEX_POINT('',#11815);
#3784=VERTEX_POINT('',#11817);
#3785=VERTEX_POINT('',#11821);
#3786=VERTEX_POINT('',#11823);
#3787=VERTEX_POINT('',#11827);
#3788=VERTEX_POINT('',#11829);
#3789=VERTEX_POINT('',#11833);
#3790=VERTEX_POINT('',#11835);
#3791=VERTEX_POINT('',#11839);
#3792=VERTEX_POINT('',#11843);
#3793=VERTEX_POINT('',#11845);
#3794=VERTEX_POINT('',#11849);
#3795=VERTEX_POINT('',#11851);
#3796=VERTEX_POINT('',#11858);
#3797=VERTEX_POINT('',#11860);
#3798=VERTEX_POINT('',#11867);
#3799=VERTEX_POINT('',#11869);
#3800=VERTEX_POINT('',#11882);
#3801=VERTEX_POINT('',#11883);
#3802=VERTEX_POINT('',#11885);
#3803=VERTEX_POINT('',#11887);
#3804=VERTEX_POINT('',#11891);
#3805=VERTEX_POINT('',#11893);
#3806=VERTEX_POINT('',#11897);
#3807=VERTEX_POINT('',#11899);
#3808=VERTEX_POINT('',#11903);
#3809=VERTEX_POINT('',#11905);
#3810=VERTEX_POINT('',#11909);
#3811=VERTEX_POINT('',#11911);
#3812=VERTEX_POINT('',#11915);
#3813=VERTEX_POINT('',#11917);
#3814=VERTEX_POINT('',#11921);
#3815=VERTEX_POINT('',#11923);
#3816=VERTEX_POINT('',#11927);
#3817=VERTEX_POINT('',#11929);
#3818=VERTEX_POINT('',#11933);
#3819=VERTEX_POINT('',#11935);
#3820=VERTEX_POINT('',#11939);
#3821=VERTEX_POINT('',#11940);
#3822=VERTEX_POINT('',#11942);
#3823=VERTEX_POINT('',#11944);
#3824=VERTEX_POINT('',#11948);
#3825=VERTEX_POINT('',#11950);
#3826=VERTEX_POINT('',#11954);
#3827=VERTEX_POINT('',#11956);
#3828=VERTEX_POINT('',#11960);
#3829=VERTEX_POINT('',#11962);
#3830=VERTEX_POINT('',#11966);
#3831=VERTEX_POINT('',#11968);
#3832=VERTEX_POINT('',#11972);
#3833=VERTEX_POINT('',#11974);
#3834=VERTEX_POINT('',#11978);
#3835=VERTEX_POINT('',#11980);
#3836=VERTEX_POINT('',#11984);
#3837=VERTEX_POINT('',#11986);
#3838=VERTEX_POINT('',#11990);
#3839=VERTEX_POINT('',#11992);
#3840=VERTEX_POINT('',#11996);
#3841=VERTEX_POINT('',#11997);
#3842=VERTEX_POINT('',#11999);
#3843=VERTEX_POINT('',#12001);
#3844=VERTEX_POINT('',#12005);
#3845=VERTEX_POINT('',#12007);
#3846=VERTEX_POINT('',#12011);
#3847=VERTEX_POINT('',#12013);
#3848=VERTEX_POINT('',#12017);
#3849=VERTEX_POINT('',#12019);
#3850=VERTEX_POINT('',#12023);
#3851=VERTEX_POINT('',#12025);
#3852=VERTEX_POINT('',#12029);
#3853=VERTEX_POINT('',#12031);
#3854=VERTEX_POINT('',#12035);
#3855=VERTEX_POINT('',#12037);
#3856=VERTEX_POINT('',#12041);
#3857=VERTEX_POINT('',#12043);
#3858=VERTEX_POINT('',#12047);
#3859=VERTEX_POINT('',#12049);
#3860=VERTEX_POINT('',#12053);
#3861=VERTEX_POINT('',#12054);
#3862=VERTEX_POINT('',#12056);
#3863=VERTEX_POINT('',#12058);
#3864=VERTEX_POINT('',#12062);
#3865=VERTEX_POINT('',#12064);
#3866=VERTEX_POINT('',#12068);
#3867=VERTEX_POINT('',#12070);
#3868=VERTEX_POINT('',#12074);
#3869=VERTEX_POINT('',#12076);
#3870=VERTEX_POINT('',#12080);
#3871=VERTEX_POINT('',#12082);
#3872=VERTEX_POINT('',#12086);
#3873=VERTEX_POINT('',#12088);
#3874=VERTEX_POINT('',#12092);
#3875=VERTEX_POINT('',#12094);
#3876=VERTEX_POINT('',#12098);
#3877=VERTEX_POINT('',#12100);
#3878=VERTEX_POINT('',#12104);
#3879=VERTEX_POINT('',#12106);
#3880=VERTEX_POINT('',#12110);
#3881=VERTEX_POINT('',#12112);
#3882=VERTEX_POINT('',#12116);
#3883=VERTEX_POINT('',#12118);
#3884=VERTEX_POINT('',#12122);
#3885=VERTEX_POINT('',#12124);
#3886=VERTEX_POINT('',#12131);
#3887=VERTEX_POINT('',#12133);
#3888=VERTEX_POINT('',#12140);
#3889=VERTEX_POINT('',#12142);
#3890=VERTEX_POINT('',#12155);
#3891=VERTEX_POINT('',#12156);
#3892=VERTEX_POINT('',#12158);
#3893=VERTEX_POINT('',#12160);
#3894=VERTEX_POINT('',#12164);
#3895=VERTEX_POINT('',#12166);
#3896=VERTEX_POINT('',#12170);
#3897=VERTEX_POINT('',#12172);
#3898=VERTEX_POINT('',#12176);
#3899=VERTEX_POINT('',#12178);
#3900=VERTEX_POINT('',#12182);
#3901=VERTEX_POINT('',#12184);
#3902=VERTEX_POINT('',#12193);
#3903=VERTEX_POINT('',#12195);
#3904=VERTEX_POINT('',#12198);
#3905=VERTEX_POINT('',#12203);
#3906=VERTEX_POINT('',#12206);
#3907=VERTEX_POINT('',#12210);
#3908=VERTEX_POINT('',#12214);
#3909=VERTEX_POINT('',#12218);
#3910=VERTEX_POINT('',#12221);
#3911=VERTEX_POINT('',#12228);
#3912=VERTEX_POINT('',#12231);
#3913=VERTEX_POINT('',#12235);
#3914=VERTEX_POINT('',#12239);
#3915=VERTEX_POINT('',#12243);
#3916=VERTEX_POINT('',#12246);
#3917=VERTEX_POINT('',#12250);
#3918=VERTEX_POINT('',#12254);
#3919=VERTEX_POINT('',#12259);
#3920=VERTEX_POINT('',#12260);
#3921=VERTEX_POINT('',#12262);
#3922=VERTEX_POINT('',#12264);
#3923=VERTEX_POINT('',#12268);
#3924=VERTEX_POINT('',#12270);
#3925=VERTEX_POINT('',#12274);
#3926=VERTEX_POINT('',#12276);
#3927=VERTEX_POINT('',#12280);
#3928=VERTEX_POINT('',#12282);
#3929=VERTEX_POINT('',#12286);
#3930=VERTEX_POINT('',#12288);
#3931=VERTEX_POINT('',#12298);
#3932=VERTEX_POINT('',#12300);
#3933=VERTEX_POINT('',#12304);
#3934=VERTEX_POINT('',#12306);
#3935=VERTEX_POINT('',#12310);
#3936=VERTEX_POINT('',#12312);
#3937=VERTEX_POINT('',#12316);
#3938=VERTEX_POINT('',#12318);
#3939=VERTEX_POINT('',#12322);
#3940=VERTEX_POINT('',#12323);
#3941=VERTEX_POINT('',#12325);
#3942=VERTEX_POINT('',#12327);
#3943=VERTEX_POINT('',#12331);
#3944=VERTEX_POINT('',#12333);
#3945=VERTEX_POINT('',#12337);
#3946=VERTEX_POINT('',#12339);
#3947=VERTEX_POINT('',#12349);
#3948=VERTEX_POINT('',#12351);
#3949=VERTEX_POINT('',#12355);
#3950=VERTEX_POINT('',#12359);
#3951=VERTEX_POINT('',#12362);
#3952=VERTEX_POINT('',#12368);
#3953=VERTEX_POINT('',#12370);
#3954=VERTEX_POINT('',#12374);
#3955=VERTEX_POINT('',#12376);
#3956=VERTEX_POINT('',#12380);
#3957=VERTEX_POINT('',#12381);
#3958=VERTEX_POINT('',#12383);
#3959=VERTEX_POINT('',#12385);
#3960=VERTEX_POINT('',#12389);
#3961=VERTEX_POINT('',#12391);
#3962=VERTEX_POINT('',#12395);
#3963=VERTEX_POINT('',#12397);
#3964=VERTEX_POINT('',#12407);
#3965=VERTEX_POINT('',#12408);
#3966=VERTEX_POINT('',#12410);
#3967=VERTEX_POINT('',#12412);
#3968=VERTEX_POINT('',#12416);
#3969=VERTEX_POINT('',#12418);
#3970=VERTEX_POINT('',#12422);
#3971=VERTEX_POINT('',#12424);
#3972=VERTEX_POINT('',#12434);
#3973=VERTEX_POINT('',#12435);
#3974=VERTEX_POINT('',#12437);
#3975=VERTEX_POINT('',#12439);
#3976=VERTEX_POINT('',#12443);
#3977=VERTEX_POINT('',#12445);
#3978=VERTEX_POINT('',#12449);
#3979=VERTEX_POINT('',#12451);
#3980=VERTEX_POINT('',#12461);
#3981=VERTEX_POINT('',#12463);
#3982=VERTEX_POINT('',#12467);
#3983=VERTEX_POINT('',#12469);
#3984=VERTEX_POINT('',#12473);
#3985=VERTEX_POINT('',#12474);
#3986=VERTEX_POINT('',#12476);
#3987=VERTEX_POINT('',#12478);
#3988=VERTEX_POINT('',#12482);
#3989=VERTEX_POINT('',#12484);
#3990=VERTEX_POINT('',#12488);
#3991=VERTEX_POINT('',#12490);
#3992=VERTEX_POINT('',#12500);
#3993=VERTEX_POINT('',#12501);
#3994=VERTEX_POINT('',#12503);
#3995=VERTEX_POINT('',#12505);
#3996=VERTEX_POINT('',#12509);
#3997=VERTEX_POINT('',#12511);
#3998=VERTEX_POINT('',#12515);
#3999=VERTEX_POINT('',#12517);
#4000=VERTEX_POINT('',#12527);
#4001=VERTEX_POINT('',#12528);
#4002=VERTEX_POINT('',#12530);
#4003=VERTEX_POINT('',#12532);
#4004=VERTEX_POINT('',#12536);
#4005=VERTEX_POINT('',#12538);
#4006=VERTEX_POINT('',#12542);
#4007=VERTEX_POINT('',#12544);
#4008=VERTEX_POINT('',#12555);
#4009=VERTEX_POINT('',#12557);
#4010=VERTEX_POINT('',#12561);
#4011=VERTEX_POINT('',#12563);
#4012=VERTEX_POINT('',#12570);
#4013=VERTEX_POINT('',#12572);
#4014=VERTEX_POINT('',#12576);
#4015=VERTEX_POINT('',#12579);
#4016=VERTEX_POINT('',#12583);
#4017=VERTEX_POINT('',#12585);
#4018=VERTEX_POINT('',#12592);
#4019=VERTEX_POINT('',#12594);
#4020=VERTEX_POINT('',#12598);
#4021=VERTEX_POINT('',#12601);
#4022=VERTEX_POINT('',#12605);
#4023=VERTEX_POINT('',#12607);
#4024=VERTEX_POINT('',#12614);
#4025=VERTEX_POINT('',#12616);
#4026=VERTEX_POINT('',#12620);
#4027=VERTEX_POINT('',#12623);
#4028=VERTEX_POINT('',#12627);
#4029=VERTEX_POINT('',#12629);
#4030=VERTEX_POINT('',#12636);
#4031=VERTEX_POINT('',#12638);
#4032=VERTEX_POINT('',#12642);
#4033=VERTEX_POINT('',#12645);
#4034=VERTEX_POINT('',#12649);
#4035=VERTEX_POINT('',#12651);
#4036=VERTEX_POINT('',#12658);
#4037=VERTEX_POINT('',#12660);
#4038=VERTEX_POINT('',#12665);
#4039=VERTEX_POINT('',#12667);
#4040=VERTEX_POINT('',#12672);
#4041=VERTEX_POINT('',#12674);
#4042=VERTEX_POINT('',#12681);
#4043=VERTEX_POINT('',#12683);
#4044=VERTEX_POINT('',#12687);
#4045=VERTEX_POINT('',#12690);
#4046=VERTEX_POINT('',#12692);
#4047=VERTEX_POINT('',#12696);
#4048=VERTEX_POINT('',#12699);
#4049=VERTEX_POINT('',#12703);
#4050=VERTEX_POINT('',#12707);
#4051=VERTEX_POINT('',#12709);
#4052=VERTEX_POINT('',#12713);
#4053=VERTEX_POINT('',#12714);
#4054=VERTEX_POINT('',#12716);
#4055=VERTEX_POINT('',#12718);
#4056=VERTEX_POINT('',#12722);
#4057=VERTEX_POINT('',#12724);
#4058=VERTEX_POINT('',#12728);
#4059=VERTEX_POINT('',#12730);
#4060=VERTEX_POINT('',#12740);
#4061=VERTEX_POINT('',#12742);
#4062=VERTEX_POINT('',#12746);
#4063=VERTEX_POINT('',#12748);
#4064=VERTEX_POINT('',#12755);
#4065=VERTEX_POINT('',#12757);
#4066=VERTEX_POINT('',#12761);
#4067=VERTEX_POINT('',#12763);
#4068=VERTEX_POINT('',#12771);
#4069=VERTEX_POINT('',#12772);
#4070=VERTEX_POINT('',#12775);
#4071=VERTEX_POINT('',#12777);
#4072=VERTEX_POINT('',#12781);
#4073=VERTEX_POINT('',#12785);
#4074=VERTEX_POINT('',#12787);
#4075=VERTEX_POINT('',#12791);
#4076=VERTEX_POINT('',#12796);
#4077=VERTEX_POINT('',#12800);
#4078=VERTEX_POINT('',#12806);
#4079=VERTEX_POINT('',#12807);
#4080=VERTEX_POINT('',#12810);
#4081=VERTEX_POINT('',#12812);
#4082=VERTEX_POINT('',#12816);
#4083=VERTEX_POINT('',#12820);
#4084=VERTEX_POINT('',#12822);
#4085=VERTEX_POINT('',#12825);
#4086=VERTEX_POINT('',#12829);
#4087=VERTEX_POINT('',#12833);
#4088=VERTEX_POINT('',#12841);
#4089=VERTEX_POINT('',#12842);
#4090=VERTEX_POINT('',#12845);
#4091=VERTEX_POINT('',#12846);
#4092=VERTEX_POINT('',#12849);
#4093=VERTEX_POINT('',#12850);
#4094=VERTEX_POINT('',#12853);
#4095=VERTEX_POINT('',#12854);
#4096=VERTEX_POINT('',#12857);
#4097=VERTEX_POINT('',#12858);
#4098=VERTEX_POINT('',#12861);
#4099=VERTEX_POINT('',#12862);
#4100=VERTEX_POINT('',#12865);
#4101=VERTEX_POINT('',#12866);
#4102=VERTEX_POINT('',#12869);
#4103=VERTEX_POINT('',#12870);
#4104=VERTEX_POINT('',#12874);
#4105=VERTEX_POINT('',#12875);
#4106=VERTEX_POINT('',#12898);
#4107=VERTEX_POINT('',#12900);
#4108=VERTEX_POINT('',#12925);
#4109=VERTEX_POINT('',#12927);
#4110=VERTEX_POINT('',#12950);
#4111=VERTEX_POINT('',#12952);
#4112=VERTEX_POINT('',#12975);
#4113=VERTEX_POINT('',#12977);
#4114=VERTEX_POINT('',#12990);
#4115=VERTEX_POINT('',#12993);
#4116=VERTEX_POINT('',#13006);
#4117=VERTEX_POINT('',#13008);
#4118=VERTEX_POINT('',#13031);
#4119=VERTEX_POINT('',#13033);
#4120=VERTEX_POINT('',#13056);
#4121=VERTEX_POINT('',#13058);
#4122=VERTEX_POINT('',#13081);
#4123=VERTEX_POINT('',#13083);
#4124=VERTEX_POINT('',#13108);
#4125=VERTEX_POINT('',#13112);
#4126=VERTEX_POINT('',#13137);
#4127=VERTEX_POINT('',#13141);
#4128=VERTEX_POINT('',#13166);
#4129=VERTEX_POINT('',#13170);
#4130=VERTEX_POINT('',#13171);
#4131=VERTEX_POINT('',#13198);
#4132=VERTEX_POINT('',#13202);
#4133=VERTEX_POINT('',#13227);
#4134=VERTEX_POINT('',#13231);
#4135=VERTEX_POINT('',#13256);
#4136=VERTEX_POINT('',#13260);
#4137=VERTEX_POINT('',#13285);
#4138=VERTEX_POINT('',#13288);
#4139=VERTEX_POINT('',#13290);
#4140=VERTEX_POINT('',#13322);
#4141=VERTEX_POINT('',#13324);
#4142=VERTEX_POINT('',#13327);
#4143=VERTEX_POINT('',#13331);
#4144=VERTEX_POINT('',#13336);
#4145=VERTEX_POINT('',#13338);
#4146=VERTEX_POINT('',#13341);
#4147=VERTEX_POINT('',#13345);
#4148=VERTEX_POINT('',#13356);
#4149=VERTEX_POINT('',#13358);
#4150=VERTEX_POINT('',#13362);
#4151=VERTEX_POINT('',#13364);
#4152=VERTEX_POINT('',#13371);
#4153=VERTEX_POINT('',#13372);
#4154=VERTEX_POINT('',#13374);
#4155=VERTEX_POINT('',#13376);
#4156=VERTEX_POINT('',#13380);
#4157=VERTEX_POINT('',#13382);
#4158=VERTEX_POINT('',#13386);
#4159=VERTEX_POINT('',#13388);
#4160=VERTEX_POINT('',#13392);
#4161=VERTEX_POINT('',#13394);
#4162=VERTEX_POINT('',#13398);
#4163=VERTEX_POINT('',#13400);
#4164=VERTEX_POINT('',#13409);
#4165=VERTEX_POINT('',#13412);
#4166=VERTEX_POINT('',#13415);
#4167=VERTEX_POINT('',#13419);
#4168=VERTEX_POINT('',#13423);
#4169=VERTEX_POINT('',#13427);
#4170=VERTEX_POINT('',#13430);
#4171=VERTEX_POINT('',#13437);
#4172=VERTEX_POINT('',#13439);
#4173=VERTEX_POINT('',#13443);
#4174=VERTEX_POINT('',#13445);
#4175=VERTEX_POINT('',#13452);
#4176=VERTEX_POINT('',#13453);
#4177=VERTEX_POINT('',#13455);
#4178=VERTEX_POINT('',#13457);
#4179=VERTEX_POINT('',#13461);
#4180=VERTEX_POINT('',#13463);
#4181=VERTEX_POINT('',#13467);
#4182=VERTEX_POINT('',#13469);
#4183=VERTEX_POINT('',#13472);
#4184=VERTEX_POINT('',#13475);
#4185=VERTEX_POINT('',#13477);
#4186=VERTEX_POINT('',#13479);
#4187=VERTEX_POINT('',#13481);
#4188=VERTEX_POINT('',#13483);
#4189=VERTEX_POINT('',#13485);
#4190=VERTEX_POINT('',#13489);
#4191=VERTEX_POINT('',#13493);
#4192=VERTEX_POINT('',#13497);
#4193=VERTEX_POINT('',#13499);
#4194=VERTEX_POINT('',#13501);
#4195=VERTEX_POINT('',#13503);
#4196=VERTEX_POINT('',#13509);
#4197=VERTEX_POINT('',#13511);
#4198=VERTEX_POINT('',#13515);
#4199=VERTEX_POINT('',#13518);
#4200=VERTEX_POINT('',#13520);
#4201=VERTEX_POINT('',#13532);
#4202=VERTEX_POINT('',#13533);
#4203=VERTEX_POINT('',#13535);
#4204=VERTEX_POINT('',#13537);
#4205=VERTEX_POINT('',#13541);
#4206=VERTEX_POINT('',#13543);
#4207=VERTEX_POINT('',#13547);
#4208=VERTEX_POINT('',#13549);
#4209=VERTEX_POINT('',#13553);
#4210=VERTEX_POINT('',#13555);
#4211=VERTEX_POINT('',#13559);
#4212=VERTEX_POINT('',#13561);
#4213=VERTEX_POINT('',#13570);
#4214=VERTEX_POINT('',#13573);
#4215=VERTEX_POINT('',#13576);
#4216=VERTEX_POINT('',#13580);
#4217=VERTEX_POINT('',#13584);
#4218=VERTEX_POINT('',#13588);
#4219=VERTEX_POINT('',#13591);
#4220=VERTEX_POINT('',#13654);
#4221=VERTEX_POINT('',#13656);
#4222=VERTEX_POINT('',#13660);
#4223=VERTEX_POINT('',#13663);
#4224=VERTEX_POINT('',#13665);
#4225=VERTEX_POINT('',#13669);
#4226=VERTEX_POINT('',#13672);
#4227=VERTEX_POINT('',#13676);
#4228=VERTEX_POINT('',#13680);
#4229=VERTEX_POINT('',#13682);
#4230=VERTEX_POINT('',#13686);
#4231=VERTEX_POINT('',#13687);
#4232=VERTEX_POINT('',#13689);
#4233=VERTEX_POINT('',#13691);
#4234=VERTEX_POINT('',#13695);
#4235=VERTEX_POINT('',#13697);
#4236=VERTEX_POINT('',#13701);
#4237=VERTEX_POINT('',#13703);
#4238=EDGE_CURVE('',#3590,#3590,#3374,.T.);
#4239=EDGE_CURVE('',#3590,#3591,#1938,.T.);
#4240=EDGE_CURVE('',#3591,#3591,#3375,.T.);
#4241=EDGE_CURVE('',#3592,#3592,#3376,.T.);
#4242=EDGE_CURVE('',#3592,#3593,#1939,.T.);
#4243=EDGE_CURVE('',#3593,#3593,#3377,.T.);
#4244=EDGE_CURVE('',#3594,#3594,#3378,.T.);
#4245=EDGE_CURVE('',#3594,#3595,#1940,.T.);
#4246=EDGE_CURVE('',#3595,#3595,#3379,.T.);
#4247=EDGE_CURVE('',#3596,#3596,#3380,.T.);
#4248=EDGE_CURVE('',#3596,#3597,#1941,.T.);
#4249=EDGE_CURVE('',#3597,#3597,#3381,.T.);
#4250=EDGE_CURVE('',#3598,#3599,#1942,.T.);
#4251=EDGE_CURVE('',#3599,#3600,#1943,.T.);
#4252=EDGE_CURVE('',#3601,#3600,#1944,.T.);
#4253=EDGE_CURVE('',#3598,#3601,#1945,.T.);
#4254=EDGE_CURVE('',#3602,#3598,#1946,.T.);
#4255=EDGE_CURVE('',#3603,#3601,#1947,.T.);
#4256=EDGE_CURVE('',#3602,#3603,#1948,.T.);
#4257=EDGE_CURVE('',#3604,#3602,#1949,.T.);
#4258=EDGE_CURVE('',#3605,#3603,#1950,.T.);
#4259=EDGE_CURVE('',#3604,#3605,#1951,.T.);
#4260=EDGE_CURVE('',#3599,#3604,#1952,.T.);
#4261=EDGE_CURVE('',#3600,#3605,#1953,.T.);
#4262=EDGE_CURVE('',#3606,#3606,#3382,.T.);
#4263=EDGE_CURVE('',#3606,#3607,#1954,.T.);
#4264=EDGE_CURVE('',#3608,#3607,#433,.T.);
#4265=EDGE_CURVE('',#3608,#3609,#1955,.T.);
#4266=EDGE_CURVE('',#3609,#3609,#3383,.T.);
#4267=EDGE_CURVE('',#3610,#3608,#434,.T.);
#4268=EDGE_CURVE('',#3607,#3610,#435,.T.);
#4269=EDGE_CURVE('',#3611,#3612,#436,.T.);
#4270=EDGE_CURVE('',#3612,#3611,#437,.T.);
#4271=EDGE_CURVE('',#3613,#3613,#3384,.T.);
#4272=EDGE_CURVE('',#3613,#3608,#1956,.T.);
#4273=EDGE_CURVE('',#3614,#3615,#1957,.T.);
#4274=EDGE_CURVE('',#3614,#3616,#1958,.T.);
#4275=EDGE_CURVE('',#3617,#3616,#1959,.T.);
#4276=EDGE_CURVE('',#3615,#3617,#1960,.T.);
#4277=EDGE_CURVE('',#3618,#3614,#1961,.T.);
#4278=EDGE_CURVE('',#3618,#3619,#1962,.T.);
#4279=EDGE_CURVE('',#3616,#3619,#1963,.T.);
#4280=EDGE_CURVE('',#3620,#3618,#1964,.T.);
#4281=EDGE_CURVE('',#3620,#3621,#1965,.T.);
#4282=EDGE_CURVE('',#3619,#3621,#1966,.T.);
#4283=EDGE_CURVE('',#3622,#3620,#1967,.T.);
#4284=EDGE_CURVE('',#3622,#3623,#1968,.T.);
#4285=EDGE_CURVE('',#3621,#3623,#1969,.T.);
#4286=EDGE_CURVE('',#3624,#3622,#1970,.T.);
#4287=EDGE_CURVE('',#3624,#3625,#1971,.T.);
#4288=EDGE_CURVE('',#3623,#3625,#1972,.T.);
#4289=EDGE_CURVE('',#3626,#3624,#1973,.T.);
#4290=EDGE_CURVE('',#3626,#3627,#1974,.T.);
#4291=EDGE_CURVE('',#3625,#3627,#1975,.T.);
#4292=EDGE_CURVE('',#3628,#3626,#1976,.T.);
#4293=EDGE_CURVE('',#3628,#3629,#1977,.T.);
#4294=EDGE_CURVE('',#3627,#3629,#1978,.T.);
#4295=EDGE_CURVE('',#3630,#3628,#1979,.T.);
#4296=EDGE_CURVE('',#3630,#3631,#1980,.T.);
#4297=EDGE_CURVE('',#3629,#3631,#1981,.T.);
#4298=EDGE_CURVE('',#3632,#3630,#1982,.T.);
#4299=EDGE_CURVE('',#3633,#3632,#1983,.T.);
#4300=EDGE_CURVE('',#3631,#3633,#1984,.T.);
#4301=EDGE_CURVE('',#3634,#3635,#1985,.T.);
#4302=EDGE_CURVE('',#3634,#3636,#1986,.T.);
#4303=EDGE_CURVE('',#3637,#3636,#1987,.T.);
#4304=EDGE_CURVE('',#3635,#3637,#1988,.T.);
#4305=EDGE_CURVE('',#3638,#3634,#1989,.T.);
#4306=EDGE_CURVE('',#3638,#3639,#1990,.T.);
#4307=EDGE_CURVE('',#3636,#3639,#1991,.T.);
#4308=EDGE_CURVE('',#3640,#3638,#1992,.T.);
#4309=EDGE_CURVE('',#3640,#3641,#1993,.T.);
#4310=EDGE_CURVE('',#3639,#3641,#1994,.T.);
#4311=EDGE_CURVE('',#3642,#3640,#1995,.T.);
#4312=EDGE_CURVE('',#3642,#3643,#1996,.T.);
#4313=EDGE_CURVE('',#3641,#3643,#1997,.T.);
#4314=EDGE_CURVE('',#3644,#3642,#1998,.T.);
#4315=EDGE_CURVE('',#3644,#3645,#1999,.T.);
#4316=EDGE_CURVE('',#3643,#3645,#2000,.T.);
#4317=EDGE_CURVE('',#3646,#3644,#2001,.T.);
#4318=EDGE_CURVE('',#3646,#3647,#2002,.T.);
#4319=EDGE_CURVE('',#3645,#3647,#2003,.T.);
#4320=EDGE_CURVE('',#3648,#3646,#2004,.T.);
#4321=EDGE_CURVE('',#3648,#3649,#2005,.T.);
#4322=EDGE_CURVE('',#3647,#3649,#2006,.T.);
#4323=EDGE_CURVE('',#3650,#3648,#2007,.T.);
#4324=EDGE_CURVE('',#3650,#3651,#2008,.T.);
#4325=EDGE_CURVE('',#3649,#3651,#2009,.T.);
#4326=EDGE_CURVE('',#3652,#3650,#2010,.T.);
#4327=EDGE_CURVE('',#3653,#3652,#2011,.T.);
#4328=EDGE_CURVE('',#3651,#3653,#2012,.T.);
#4329=EDGE_CURVE('',#3654,#3655,#2013,.T.);
#4330=EDGE_CURVE('',#3654,#3656,#2014,.T.);
#4331=EDGE_CURVE('',#3657,#3656,#2015,.T.);
#4332=EDGE_CURVE('',#3655,#3657,#2016,.T.);
#4333=EDGE_CURVE('',#3658,#3654,#2017,.T.);
#4334=EDGE_CURVE('',#3658,#3659,#2018,.T.);
#4335=EDGE_CURVE('',#3656,#3659,#2019,.T.);
#4336=EDGE_CURVE('',#3660,#3658,#2020,.T.);
#4337=EDGE_CURVE('',#3660,#3661,#2021,.T.);
#4338=EDGE_CURVE('',#3659,#3661,#2022,.T.);
#4339=EDGE_CURVE('',#3662,#3660,#2023,.T.);
#4340=EDGE_CURVE('',#3662,#3663,#2024,.T.);
#4341=EDGE_CURVE('',#3661,#3663,#2025,.T.);
#4342=EDGE_CURVE('',#3664,#3662,#2026,.T.);
#4343=EDGE_CURVE('',#3664,#3665,#2027,.T.);
#4344=EDGE_CURVE('',#3663,#3665,#2028,.T.);
#4345=EDGE_CURVE('',#3666,#3664,#2029,.T.);
#4346=EDGE_CURVE('',#3666,#3667,#2030,.T.);
#4347=EDGE_CURVE('',#3665,#3667,#2031,.T.);
#4348=EDGE_CURVE('',#3668,#3666,#2032,.T.);
#4349=EDGE_CURVE('',#3668,#3669,#2033,.T.);
#4350=EDGE_CURVE('',#3667,#3669,#2034,.T.);
#4351=EDGE_CURVE('',#3670,#3668,#2035,.T.);
#4352=EDGE_CURVE('',#3670,#3671,#2036,.T.);
#4353=EDGE_CURVE('',#3669,#3671,#2037,.T.);
#4354=EDGE_CURVE('',#3672,#3670,#2038,.T.);
#4355=EDGE_CURVE('',#3673,#3672,#2039,.T.);
#4356=EDGE_CURVE('',#3671,#3673,#2040,.T.);
#4357=EDGE_CURVE('',#3674,#3675,#2041,.T.);
#4358=EDGE_CURVE('',#3674,#3676,#2042,.T.);
#4359=EDGE_CURVE('',#3677,#3676,#2043,.T.);
#4360=EDGE_CURVE('',#3675,#3677,#2044,.T.);
#4361=EDGE_CURVE('',#3678,#3674,#2045,.T.);
#4362=EDGE_CURVE('',#3678,#3679,#2046,.T.);
#4363=EDGE_CURVE('',#3676,#3679,#2047,.T.);
#4364=EDGE_CURVE('',#3680,#3678,#2048,.T.);
#4365=EDGE_CURVE('',#3680,#3681,#2049,.T.);
#4366=EDGE_CURVE('',#3679,#3681,#2050,.T.);
#4367=EDGE_CURVE('',#3682,#3680,#2051,.T.);
#4368=EDGE_CURVE('',#3682,#3683,#2052,.T.);
#4369=EDGE_CURVE('',#3681,#3683,#2053,.T.);
#4370=EDGE_CURVE('',#3684,#3682,#2054,.T.);
#4371=EDGE_CURVE('',#3684,#3685,#2055,.T.);
#4372=EDGE_CURVE('',#3683,#3685,#2056,.T.);
#4373=EDGE_CURVE('',#3686,#3684,#2057,.T.);
#4374=EDGE_CURVE('',#3686,#3687,#2058,.T.);
#4375=EDGE_CURVE('',#3685,#3687,#2059,.T.);
#4376=EDGE_CURVE('',#3688,#3686,#2060,.T.);
#4377=EDGE_CURVE('',#3688,#3689,#2061,.T.);
#4378=EDGE_CURVE('',#3687,#3689,#2062,.T.);
#4379=EDGE_CURVE('',#3690,#3688,#2063,.T.);
#4380=EDGE_CURVE('',#3690,#3691,#2064,.T.);
#4381=EDGE_CURVE('',#3689,#3691,#2065,.T.);
#4382=EDGE_CURVE('',#3692,#3690,#2066,.T.);
#4383=EDGE_CURVE('',#3693,#3692,#2067,.T.);
#4384=EDGE_CURVE('',#3691,#3693,#2068,.T.);
#4385=EDGE_CURVE('',#3612,#3694,#2069,.T.);
#4386=EDGE_CURVE('',#3694,#3694,#3385,.T.);
#4387=EDGE_CURVE('',#3632,#3695,#2070,.T.);
#4388=EDGE_CURVE('',#3695,#3696,#2071,.T.);
#4389=EDGE_CURVE('',#3633,#3696,#2072,.T.);
#4390=EDGE_CURVE('',#3697,#3617,#2073,.T.);
#4391=EDGE_CURVE('',#3698,#3697,#2074,.T.);
#4392=EDGE_CURVE('',#3698,#3615,#2075,.T.);
#4393=EDGE_CURVE('',#3652,#3698,#2076,.T.);
#4394=EDGE_CURVE('',#3653,#3697,#2077,.T.);
#4395=EDGE_CURVE('',#3699,#3637,#2078,.T.);
#4396=EDGE_CURVE('',#3700,#3699,#2079,.T.);
#4397=EDGE_CURVE('',#3700,#3635,#2080,.T.);
#4398=EDGE_CURVE('',#3672,#3700,#2081,.T.);
#4399=EDGE_CURVE('',#3673,#3699,#2082,.T.);
#4400=EDGE_CURVE('',#3701,#3657,#2083,.T.);
#4401=EDGE_CURVE('',#3702,#3701,#2084,.T.);
#4402=EDGE_CURVE('',#3702,#3655,#2085,.T.);
#4403=EDGE_CURVE('',#3692,#3702,#2086,.T.);
#4404=EDGE_CURVE('',#3693,#3701,#2087,.T.);
#4405=EDGE_CURVE('',#3696,#3677,#2088,.T.);
#4406=EDGE_CURVE('',#3695,#3675,#2089,.T.);
#4407=EDGE_CURVE('',#3703,#3703,#3386,.T.);
#4408=EDGE_CURVE('',#3703,#3704,#2090,.T.);
#4409=EDGE_CURVE('',#3705,#3704,#438,.T.);
#4410=EDGE_CURVE('',#3705,#3706,#2091,.T.);
#4411=EDGE_CURVE('',#3706,#3706,#3387,.T.);
#4412=EDGE_CURVE('',#3707,#3705,#439,.T.);
#4413=EDGE_CURVE('',#3704,#3707,#440,.T.);
#4414=EDGE_CURVE('',#3708,#3709,#441,.T.);
#4415=EDGE_CURVE('',#3709,#3708,#442,.T.);
#4416=EDGE_CURVE('',#3710,#3710,#3388,.T.);
#4417=EDGE_CURVE('',#3710,#3705,#2092,.T.);
#4418=EDGE_CURVE('',#3711,#3712,#2093,.T.);
#4419=EDGE_CURVE('',#3711,#3713,#2094,.T.);
#4420=EDGE_CURVE('',#3714,#3713,#2095,.T.);
#4421=EDGE_CURVE('',#3712,#3714,#2096,.T.);
#4422=EDGE_CURVE('',#3715,#3711,#2097,.T.);
#4423=EDGE_CURVE('',#3715,#3716,#2098,.T.);
#4424=EDGE_CURVE('',#3713,#3716,#2099,.T.);
#4425=EDGE_CURVE('',#3717,#3715,#2100,.T.);
#4426=EDGE_CURVE('',#3717,#3718,#2101,.T.);
#4427=EDGE_CURVE('',#3716,#3718,#2102,.T.);
#4428=EDGE_CURVE('',#3719,#3717,#2103,.T.);
#4429=EDGE_CURVE('',#3719,#3720,#2104,.T.);
#4430=EDGE_CURVE('',#3718,#3720,#2105,.T.);
#4431=EDGE_CURVE('',#3721,#3719,#2106,.T.);
#4432=EDGE_CURVE('',#3721,#3722,#2107,.T.);
#4433=EDGE_CURVE('',#3720,#3722,#2108,.T.);
#4434=EDGE_CURVE('',#3723,#3721,#2109,.T.);
#4435=EDGE_CURVE('',#3723,#3724,#2110,.T.);
#4436=EDGE_CURVE('',#3722,#3724,#2111,.T.);
#4437=EDGE_CURVE('',#3725,#3723,#2112,.T.);
#4438=EDGE_CURVE('',#3725,#3726,#2113,.T.);
#4439=EDGE_CURVE('',#3724,#3726,#2114,.T.);
#4440=EDGE_CURVE('',#3727,#3725,#2115,.T.);
#4441=EDGE_CURVE('',#3727,#3728,#2116,.T.);
#4442=EDGE_CURVE('',#3726,#3728,#2117,.T.);
#4443=EDGE_CURVE('',#3729,#3727,#2118,.T.);
#4444=EDGE_CURVE('',#3730,#3729,#2119,.T.);
#4445=EDGE_CURVE('',#3728,#3730,#2120,.T.);
#4446=EDGE_CURVE('',#3731,#3732,#2121,.T.);
#4447=EDGE_CURVE('',#3731,#3733,#2122,.T.);
#4448=EDGE_CURVE('',#3734,#3733,#2123,.T.);
#4449=EDGE_CURVE('',#3732,#3734,#2124,.T.);
#4450=EDGE_CURVE('',#3735,#3731,#2125,.T.);
#4451=EDGE_CURVE('',#3735,#3736,#2126,.T.);
#4452=EDGE_CURVE('',#3733,#3736,#2127,.T.);
#4453=EDGE_CURVE('',#3737,#3735,#2128,.T.);
#4454=EDGE_CURVE('',#3737,#3738,#2129,.T.);
#4455=EDGE_CURVE('',#3736,#3738,#2130,.T.);
#4456=EDGE_CURVE('',#3739,#3737,#2131,.T.);
#4457=EDGE_CURVE('',#3739,#3740,#2132,.T.);
#4458=EDGE_CURVE('',#3738,#3740,#2133,.T.);
#4459=EDGE_CURVE('',#3741,#3739,#2134,.T.);
#4460=EDGE_CURVE('',#3741,#3742,#2135,.T.);
#4461=EDGE_CURVE('',#3740,#3742,#2136,.T.);
#4462=EDGE_CURVE('',#3743,#3741,#2137,.T.);
#4463=EDGE_CURVE('',#3743,#3744,#2138,.T.);
#4464=EDGE_CURVE('',#3742,#3744,#2139,.T.);
#4465=EDGE_CURVE('',#3745,#3743,#2140,.T.);
#4466=EDGE_CURVE('',#3745,#3746,#2141,.T.);
#4467=EDGE_CURVE('',#3744,#3746,#2142,.T.);
#4468=EDGE_CURVE('',#3747,#3745,#2143,.T.);
#4469=EDGE_CURVE('',#3747,#3748,#2144,.T.);
#4470=EDGE_CURVE('',#3746,#3748,#2145,.T.);
#4471=EDGE_CURVE('',#3749,#3747,#2146,.T.);
#4472=EDGE_CURVE('',#3750,#3749,#2147,.T.);
#4473=EDGE_CURVE('',#3748,#3750,#2148,.T.);
#4474=EDGE_CURVE('',#3751,#3752,#2149,.T.);
#4475=EDGE_CURVE('',#3751,#3753,#2150,.T.);
#4476=EDGE_CURVE('',#3754,#3753,#2151,.T.);
#4477=EDGE_CURVE('',#3752,#3754,#2152,.T.);
#4478=EDGE_CURVE('',#3755,#3751,#2153,.T.);
#4479=EDGE_CURVE('',#3755,#3756,#2154,.T.);
#4480=EDGE_CURVE('',#3753,#3756,#2155,.T.);
#4481=EDGE_CURVE('',#3757,#3755,#2156,.T.);
#4482=EDGE_CURVE('',#3757,#3758,#2157,.T.);
#4483=EDGE_CURVE('',#3756,#3758,#2158,.T.);
#4484=EDGE_CURVE('',#3759,#3757,#2159,.T.);
#4485=EDGE_CURVE('',#3759,#3760,#2160,.T.);
#4486=EDGE_CURVE('',#3758,#3760,#2161,.T.);
#4487=EDGE_CURVE('',#3761,#3759,#2162,.T.);
#4488=EDGE_CURVE('',#3761,#3762,#2163,.T.);
#4489=EDGE_CURVE('',#3760,#3762,#2164,.T.);
#4490=EDGE_CURVE('',#3763,#3761,#2165,.T.);
#4491=EDGE_CURVE('',#3763,#3764,#2166,.T.);
#4492=EDGE_CURVE('',#3762,#3764,#2167,.T.);
#4493=EDGE_CURVE('',#3765,#3763,#2168,.T.);
#4494=EDGE_CURVE('',#3765,#3766,#2169,.T.);
#4495=EDGE_CURVE('',#3764,#3766,#2170,.T.);
#4496=EDGE_CURVE('',#3767,#3765,#2171,.T.);
#4497=EDGE_CURVE('',#3767,#3768,#2172,.T.);
#4498=EDGE_CURVE('',#3766,#3768,#2173,.T.);
#4499=EDGE_CURVE('',#3769,#3767,#2174,.T.);
#4500=EDGE_CURVE('',#3770,#3769,#2175,.T.);
#4501=EDGE_CURVE('',#3768,#3770,#2176,.T.);
#4502=EDGE_CURVE('',#3771,#3772,#2177,.T.);
#4503=EDGE_CURVE('',#3771,#3773,#2178,.T.);
#4504=EDGE_CURVE('',#3774,#3773,#2179,.T.);
#4505=EDGE_CURVE('',#3772,#3774,#2180,.T.);
#4506=EDGE_CURVE('',#3775,#3771,#2181,.T.);
#4507=EDGE_CURVE('',#3775,#3776,#2182,.T.);
#4508=EDGE_CURVE('',#3773,#3776,#2183,.T.);
#4509=EDGE_CURVE('',#3777,#3775,#2184,.T.);
#4510=EDGE_CURVE('',#3777,#3778,#2185,.T.);
#4511=EDGE_CURVE('',#3776,#3778,#2186,.T.);
#4512=EDGE_CURVE('',#3779,#3777,#2187,.T.);
#4513=EDGE_CURVE('',#3779,#3780,#2188,.T.);
#4514=EDGE_CURVE('',#3778,#3780,#2189,.T.);
#4515=EDGE_CURVE('',#3781,#3779,#2190,.T.);
#4516=EDGE_CURVE('',#3781,#3782,#2191,.T.);
#4517=EDGE_CURVE('',#3780,#3782,#2192,.T.);
#4518=EDGE_CURVE('',#3783,#3781,#2193,.T.);
#4519=EDGE_CURVE('',#3783,#3784,#2194,.T.);
#4520=EDGE_CURVE('',#3782,#3784,#2195,.T.);
#4521=EDGE_CURVE('',#3785,#3783,#2196,.T.);
#4522=EDGE_CURVE('',#3785,#3786,#2197,.T.);
#4523=EDGE_CURVE('',#3784,#3786,#2198,.T.);
#4524=EDGE_CURVE('',#3787,#3785,#2199,.T.);
#4525=EDGE_CURVE('',#3787,#3788,#2200,.T.);
#4526=EDGE_CURVE('',#3786,#3788,#2201,.T.);
#4527=EDGE_CURVE('',#3789,#3787,#2202,.T.);
#4528=EDGE_CURVE('',#3790,#3789,#2203,.T.);
#4529=EDGE_CURVE('',#3788,#3790,#2204,.T.);
#4530=EDGE_CURVE('',#3709,#3791,#2205,.T.);
#4531=EDGE_CURVE('',#3791,#3791,#3389,.T.);
#4532=EDGE_CURVE('',#3729,#3792,#2206,.T.);
#4533=EDGE_CURVE('',#3792,#3793,#2207,.T.);
#4534=EDGE_CURVE('',#3730,#3793,#2208,.T.);
#4535=EDGE_CURVE('',#3794,#3714,#2209,.T.);
#4536=EDGE_CURVE('',#3795,#3794,#2210,.T.);
#4537=EDGE_CURVE('',#3795,#3712,#2211,.T.);
#4538=EDGE_CURVE('',#3749,#3795,#2212,.T.);
#4539=EDGE_CURVE('',#3750,#3794,#2213,.T.);
#4540=EDGE_CURVE('',#3796,#3734,#2214,.T.);
#4541=EDGE_CURVE('',#3797,#3796,#2215,.T.);
#4542=EDGE_CURVE('',#3797,#3732,#2216,.T.);
#4543=EDGE_CURVE('',#3769,#3797,#2217,.T.);
#4544=EDGE_CURVE('',#3770,#3796,#2218,.T.);
#4545=EDGE_CURVE('',#3798,#3754,#2219,.T.);
#4546=EDGE_CURVE('',#3799,#3798,#2220,.T.);
#4547=EDGE_CURVE('',#3799,#3752,#2221,.T.);
#4548=EDGE_CURVE('',#3789,#3799,#2222,.T.);
#4549=EDGE_CURVE('',#3790,#3798,#2223,.T.);
#4550=EDGE_CURVE('',#3793,#3774,#2224,.T.);
#4551=EDGE_CURVE('',#3792,#3772,#2225,.T.);
#4552=EDGE_CURVE('',#3800,#3801,#2226,.T.);
#4553=EDGE_CURVE('',#3800,#3802,#2227,.T.);
#4554=EDGE_CURVE('',#3803,#3802,#2228,.T.);
#4555=EDGE_CURVE('',#3801,#3803,#2229,.T.);
#4556=EDGE_CURVE('',#3804,#3800,#2230,.T.);
#4557=EDGE_CURVE('',#3804,#3805,#2231,.T.);
#4558=EDGE_CURVE('',#3802,#3805,#2232,.T.);
#4559=EDGE_CURVE('',#3806,#3804,#2233,.T.);
#4560=EDGE_CURVE('',#3806,#3807,#2234,.T.);
#4561=EDGE_CURVE('',#3805,#3807,#2235,.T.);
#4562=EDGE_CURVE('',#3808,#3806,#2236,.T.);
#4563=EDGE_CURVE('',#3808,#3809,#2237,.T.);
#4564=EDGE_CURVE('',#3807,#3809,#2238,.T.);
#4565=EDGE_CURVE('',#3810,#3808,#2239,.T.);
#4566=EDGE_CURVE('',#3810,#3811,#2240,.T.);
#4567=EDGE_CURVE('',#3809,#3811,#2241,.T.);
#4568=EDGE_CURVE('',#3812,#3810,#2242,.T.);
#4569=EDGE_CURVE('',#3812,#3813,#2243,.T.);
#4570=EDGE_CURVE('',#3811,#3813,#2244,.T.);
#4571=EDGE_CURVE('',#3814,#3812,#2245,.T.);
#4572=EDGE_CURVE('',#3814,#3815,#2246,.T.);
#4573=EDGE_CURVE('',#3813,#3815,#2247,.T.);
#4574=EDGE_CURVE('',#3816,#3814,#2248,.T.);
#4575=EDGE_CURVE('',#3816,#3817,#2249,.T.);
#4576=EDGE_CURVE('',#3815,#3817,#2250,.T.);
#4577=EDGE_CURVE('',#3818,#3816,#2251,.T.);
#4578=EDGE_CURVE('',#3819,#3818,#2252,.T.);
#4579=EDGE_CURVE('',#3817,#3819,#2253,.T.);
#4580=EDGE_CURVE('',#3820,#3821,#2254,.T.);
#4581=EDGE_CURVE('',#3820,#3822,#2255,.T.);
#4582=EDGE_CURVE('',#3823,#3822,#2256,.T.);
#4583=EDGE_CURVE('',#3821,#3823,#2257,.T.);
#4584=EDGE_CURVE('',#3824,#3820,#2258,.T.);
#4585=EDGE_CURVE('',#3824,#3825,#2259,.T.);
#4586=EDGE_CURVE('',#3822,#3825,#2260,.T.);
#4587=EDGE_CURVE('',#3826,#3824,#2261,.T.);
#4588=EDGE_CURVE('',#3826,#3827,#2262,.T.);
#4589=EDGE_CURVE('',#3825,#3827,#2263,.T.);
#4590=EDGE_CURVE('',#3828,#3826,#2264,.T.);
#4591=EDGE_CURVE('',#3828,#3829,#2265,.T.);
#4592=EDGE_CURVE('',#3827,#3829,#2266,.T.);
#4593=EDGE_CURVE('',#3830,#3828,#2267,.T.);
#4594=EDGE_CURVE('',#3830,#3831,#2268,.T.);
#4595=EDGE_CURVE('',#3829,#3831,#2269,.T.);
#4596=EDGE_CURVE('',#3832,#3830,#2270,.T.);
#4597=EDGE_CURVE('',#3832,#3833,#2271,.T.);
#4598=EDGE_CURVE('',#3831,#3833,#2272,.T.);
#4599=EDGE_CURVE('',#3834,#3832,#2273,.T.);
#4600=EDGE_CURVE('',#3834,#3835,#2274,.T.);
#4601=EDGE_CURVE('',#3833,#3835,#2275,.T.);
#4602=EDGE_CURVE('',#3836,#3834,#2276,.T.);
#4603=EDGE_CURVE('',#3836,#3837,#2277,.T.);
#4604=EDGE_CURVE('',#3835,#3837,#2278,.T.);
#4605=EDGE_CURVE('',#3838,#3836,#2279,.T.);
#4606=EDGE_CURVE('',#3839,#3838,#2280,.T.);
#4607=EDGE_CURVE('',#3837,#3839,#2281,.T.);
#4608=EDGE_CURVE('',#3840,#3841,#2282,.T.);
#4609=EDGE_CURVE('',#3840,#3842,#2283,.T.);
#4610=EDGE_CURVE('',#3843,#3842,#2284,.T.);
#4611=EDGE_CURVE('',#3841,#3843,#2285,.T.);
#4612=EDGE_CURVE('',#3844,#3840,#2286,.T.);
#4613=EDGE_CURVE('',#3844,#3845,#2287,.T.);
#4614=EDGE_CURVE('',#3842,#3845,#2288,.T.);
#4615=EDGE_CURVE('',#3846,#3844,#2289,.T.);
#4616=EDGE_CURVE('',#3846,#3847,#2290,.T.);
#4617=EDGE_CURVE('',#3845,#3847,#2291,.T.);
#4618=EDGE_CURVE('',#3848,#3846,#2292,.T.);
#4619=EDGE_CURVE('',#3848,#3849,#2293,.T.);
#4620=EDGE_CURVE('',#3847,#3849,#2294,.T.);
#4621=EDGE_CURVE('',#3850,#3848,#2295,.T.);
#4622=EDGE_CURVE('',#3850,#3851,#2296,.T.);
#4623=EDGE_CURVE('',#3849,#3851,#2297,.T.);
#4624=EDGE_CURVE('',#3852,#3850,#2298,.T.);
#4625=EDGE_CURVE('',#3852,#3853,#2299,.T.);
#4626=EDGE_CURVE('',#3851,#3853,#2300,.T.);
#4627=EDGE_CURVE('',#3854,#3852,#2301,.T.);
#4628=EDGE_CURVE('',#3854,#3855,#2302,.T.);
#4629=EDGE_CURVE('',#3853,#3855,#2303,.T.);
#4630=EDGE_CURVE('',#3856,#3854,#2304,.T.);
#4631=EDGE_CURVE('',#3856,#3857,#2305,.T.);
#4632=EDGE_CURVE('',#3855,#3857,#2306,.T.);
#4633=EDGE_CURVE('',#3858,#3856,#2307,.T.);
#4634=EDGE_CURVE('',#3859,#3858,#2308,.T.);
#4635=EDGE_CURVE('',#3857,#3859,#2309,.T.);
#4636=EDGE_CURVE('',#3860,#3861,#2310,.T.);
#4637=EDGE_CURVE('',#3860,#3862,#2311,.T.);
#4638=EDGE_CURVE('',#3863,#3862,#2312,.T.);
#4639=EDGE_CURVE('',#3861,#3863,#2313,.T.);
#4640=EDGE_CURVE('',#3864,#3860,#2314,.T.);
#4641=EDGE_CURVE('',#3864,#3865,#2315,.T.);
#4642=EDGE_CURVE('',#3862,#3865,#2316,.T.);
#4643=EDGE_CURVE('',#3866,#3864,#2317,.T.);
#4644=EDGE_CURVE('',#3866,#3867,#2318,.T.);
#4645=EDGE_CURVE('',#3865,#3867,#2319,.T.);
#4646=EDGE_CURVE('',#3868,#3866,#2320,.T.);
#4647=EDGE_CURVE('',#3868,#3869,#2321,.T.);
#4648=EDGE_CURVE('',#3867,#3869,#2322,.T.);
#4649=EDGE_CURVE('',#3870,#3868,#2323,.T.);
#4650=EDGE_CURVE('',#3870,#3871,#2324,.T.);
#4651=EDGE_CURVE('',#3869,#3871,#2325,.T.);
#4652=EDGE_CURVE('',#3872,#3870,#2326,.T.);
#4653=EDGE_CURVE('',#3872,#3873,#2327,.T.);
#4654=EDGE_CURVE('',#3871,#3873,#2328,.T.);
#4655=EDGE_CURVE('',#3874,#3872,#2329,.T.);
#4656=EDGE_CURVE('',#3874,#3875,#2330,.T.);
#4657=EDGE_CURVE('',#3873,#3875,#2331,.T.);
#4658=EDGE_CURVE('',#3876,#3874,#2332,.T.);
#4659=EDGE_CURVE('',#3876,#3877,#2333,.T.);
#4660=EDGE_CURVE('',#3875,#3877,#2334,.T.);
#4661=EDGE_CURVE('',#3878,#3876,#2335,.T.);
#4662=EDGE_CURVE('',#3879,#3878,#2336,.T.);
#4663=EDGE_CURVE('',#3877,#3879,#2337,.T.);
#4664=EDGE_CURVE('',#3880,#3880,#3390,.T.);
#4665=EDGE_CURVE('',#3880,#3881,#2338,.T.);
#4666=EDGE_CURVE('',#3881,#3881,#3391,.T.);
#4667=EDGE_CURVE('',#3818,#3882,#2339,.T.);
#4668=EDGE_CURVE('',#3882,#3883,#2340,.T.);
#4669=EDGE_CURVE('',#3819,#3883,#2341,.T.);
#4670=EDGE_CURVE('',#3884,#3803,#2342,.T.);
#4671=EDGE_CURVE('',#3885,#3884,#2343,.T.);
#4672=EDGE_CURVE('',#3885,#3801,#2344,.T.);
#4673=EDGE_CURVE('',#3838,#3885,#2345,.T.);
#4674=EDGE_CURVE('',#3839,#3884,#2346,.T.);
#4675=EDGE_CURVE('',#3886,#3823,#2347,.T.);
#4676=EDGE_CURVE('',#3887,#3886,#2348,.T.);
#4677=EDGE_CURVE('',#3887,#3821,#2349,.T.);
#4678=EDGE_CURVE('',#3858,#3887,#2350,.T.);
#4679=EDGE_CURVE('',#3859,#3886,#2351,.T.);
#4680=EDGE_CURVE('',#3888,#3843,#2352,.T.);
#4681=EDGE_CURVE('',#3889,#3888,#2353,.T.);
#4682=EDGE_CURVE('',#3889,#3841,#2354,.T.);
#4683=EDGE_CURVE('',#3878,#3889,#2355,.T.);
#4684=EDGE_CURVE('',#3879,#3888,#2356,.T.);
#4685=EDGE_CURVE('',#3883,#3863,#2357,.T.);
#4686=EDGE_CURVE('',#3882,#3861,#2358,.T.);
#4687=EDGE_CURVE('',#3890,#3891,#2359,.T.);
#4688=EDGE_CURVE('',#3891,#3892,#2360,.T.);
#4689=EDGE_CURVE('',#3892,#3893,#2361,.T.);
#4690=EDGE_CURVE('',#3890,#3893,#2362,.T.);
#4691=EDGE_CURVE('',#3891,#3894,#2363,.T.);
#4692=EDGE_CURVE('',#3894,#3895,#2364,.T.);
#4693=EDGE_CURVE('',#3895,#3892,#2365,.T.);
#4694=EDGE_CURVE('',#3894,#3896,#2366,.T.);
#4695=EDGE_CURVE('',#3896,#3897,#2367,.T.);
#4696=EDGE_CURVE('',#3897,#3895,#2368,.T.);
#4697=EDGE_CURVE('',#3896,#3898,#2369,.T.);
#4698=EDGE_CURVE('',#3898,#3899,#2370,.T.);
#4699=EDGE_CURVE('',#3899,#3897,#2371,.T.);
#4700=EDGE_CURVE('',#3898,#3900,#2372,.T.);
#4701=EDGE_CURVE('',#3900,#3901,#2373,.T.);
#4702=EDGE_CURVE('',#3901,#3899,#2374,.T.);
#4703=EDGE_CURVE('',#3900,#3890,#2375,.T.);
#4704=EDGE_CURVE('',#3893,#3901,#2376,.T.);
#4705=EDGE_CURVE('',#3902,#3902,#3392,.T.);
#4706=EDGE_CURVE('',#3903,#3903,#3393,.T.);
#4707=EDGE_CURVE('',#3902,#3904,#2377,.T.);
#4708=EDGE_CURVE('',#3904,#3904,#3394,.T.);
#4709=EDGE_CURVE('',#3905,#3905,#3395,.T.);
#4710=EDGE_CURVE('',#3906,#3906,#3396,.T.);
#4711=EDGE_CURVE('',#3906,#3905,#2378,.T.);
#4712=EDGE_CURVE('',#3907,#3907,#3397,.T.);
#4713=EDGE_CURVE('',#3907,#3906,#2379,.T.);
#4714=EDGE_CURVE('',#3908,#3908,#3398,.T.);
#4715=EDGE_CURVE('',#3908,#3907,#2380,.T.);
#4716=EDGE_CURVE('',#3909,#3909,#3399,.T.);
#4717=EDGE_CURVE('',#3910,#3910,#3400,.F.);
#4718=EDGE_CURVE('',#3910,#3909,#2381,.T.);
#4719=EDGE_CURVE('',#3903,#3910,#2382,.T.);
#4720=EDGE_CURVE('',#3911,#3911,#3401,.T.);
#4721=EDGE_CURVE('',#3912,#3912,#3402,.T.);
#4722=EDGE_CURVE('',#3912,#3911,#2383,.T.);
#4723=EDGE_CURVE('',#3913,#3913,#3403,.T.);
#4724=EDGE_CURVE('',#3913,#3912,#2384,.T.);
#4725=EDGE_CURVE('',#3914,#3914,#3404,.T.);
#4726=EDGE_CURVE('',#3914,#3913,#2385,.T.);
#4727=EDGE_CURVE('',#3915,#3915,#3405,.T.);
#4728=EDGE_CURVE('',#3916,#3916,#3406,.F.);
#4729=EDGE_CURVE('',#3916,#3915,#2386,.T.);
#4730=EDGE_CURVE('',#3917,#3917,#3407,.F.);
#4731=EDGE_CURVE('',#3917,#3916,#2387,.T.);
#4732=EDGE_CURVE('',#3918,#3918,#3408,.T.);
#4733=EDGE_CURVE('',#3918,#3917,#2388,.T.);
#4734=EDGE_CURVE('',#3919,#3920,#2389,.T.);
#4735=EDGE_CURVE('',#3920,#3921,#2390,.T.);
#4736=EDGE_CURVE('',#3921,#3922,#2391,.T.);
#4737=EDGE_CURVE('',#3919,#3922,#2392,.T.);
#4738=EDGE_CURVE('',#3920,#3923,#2393,.T.);
#4739=EDGE_CURVE('',#3923,#3924,#2394,.T.);
#4740=EDGE_CURVE('',#3924,#3921,#2395,.T.);
#4741=EDGE_CURVE('',#3923,#3925,#2396,.T.);
#4742=EDGE_CURVE('',#3925,#3926,#2397,.T.);
#4743=EDGE_CURVE('',#3926,#3924,#2398,.T.);
#4744=EDGE_CURVE('',#3925,#3927,#2399,.T.);
#4745=EDGE_CURVE('',#3927,#3928,#2400,.T.);
#4746=EDGE_CURVE('',#3928,#3926,#2401,.T.);
#4747=EDGE_CURVE('',#3927,#3929,#2402,.T.);
#4748=EDGE_CURVE('',#3929,#3930,#2403,.T.);
#4749=EDGE_CURVE('',#3930,#3928,#2404,.T.);
#4750=EDGE_CURVE('',#3929,#3919,#2405,.T.);
#4751=EDGE_CURVE('',#3922,#3930,#2406,.T.);
#4752=EDGE_CURVE('',#3931,#3931,#3409,.T.);
#4753=EDGE_CURVE('',#3931,#3932,#2407,.T.);
#4754=EDGE_CURVE('',#3932,#3932,#3410,.T.);
#4755=EDGE_CURVE('',#3933,#3933,#3411,.T.);
#4756=EDGE_CURVE('',#3933,#3934,#2408,.T.);
#4757=EDGE_CURVE('',#3934,#3934,#3412,.T.);
#4758=EDGE_CURVE('',#3935,#3935,#3413,.T.);
#4759=EDGE_CURVE('',#3935,#3936,#2409,.T.);
#4760=EDGE_CURVE('',#3936,#3936,#3414,.T.);
#4761=EDGE_CURVE('',#3937,#3937,#3415,.T.);
#4762=EDGE_CURVE('',#3937,#3938,#2410,.T.);
#4763=EDGE_CURVE('',#3938,#3938,#3416,.T.);
#4764=EDGE_CURVE('',#3939,#3940,#2411,.T.);
#4765=EDGE_CURVE('',#3940,#3941,#2412,.T.);
#4766=EDGE_CURVE('',#3942,#3941,#2413,.T.);
#4767=EDGE_CURVE('',#3939,#3942,#2414,.T.);
#4768=EDGE_CURVE('',#3943,#3939,#2415,.T.);
#4769=EDGE_CURVE('',#3944,#3942,#2416,.T.);
#4770=EDGE_CURVE('',#3943,#3944,#2417,.T.);
#4771=EDGE_CURVE('',#3945,#3943,#2418,.T.);
#4772=EDGE_CURVE('',#3946,#3944,#2419,.T.);
#4773=EDGE_CURVE('',#3945,#3946,#2420,.T.);
#4774=EDGE_CURVE('',#3940,#3945,#2421,.T.);
#4775=EDGE_CURVE('',#3941,#3946,#2422,.T.);
#4776=EDGE_CURVE('',#3947,#3947,#3417,.T.);
#4777=EDGE_CURVE('',#3947,#3948,#2423,.T.);
#4778=EDGE_CURVE('',#3948,#3948,#3418,.T.);
#4779=EDGE_CURVE('',#3948,#3949,#2424,.T.);
#4780=EDGE_CURVE('',#3949,#3949,#3419,.T.);
#4781=EDGE_CURVE('',#3950,#3950,#3420,.T.);
#4782=EDGE_CURVE('',#3950,#3951,#2425,.T.);
#4783=EDGE_CURVE('',#3951,#3951,#3421,.T.);
#4784=EDGE_CURVE('',#3952,#3952,#3422,.T.);
#4785=EDGE_CURVE('',#3952,#3953,#2426,.T.);
#4786=EDGE_CURVE('',#3953,#3953,#3423,.T.);
#4787=EDGE_CURVE('',#3954,#3954,#3424,.T.);
#4788=EDGE_CURVE('',#3954,#3955,#2427,.T.);
#4789=EDGE_CURVE('',#3955,#3955,#3425,.T.);
#4790=EDGE_CURVE('',#3956,#3957,#2428,.T.);
#4791=EDGE_CURVE('',#3957,#3958,#2429,.T.);
#4792=EDGE_CURVE('',#3959,#3958,#2430,.T.);
#4793=EDGE_CURVE('',#3956,#3959,#2431,.T.);
#4794=EDGE_CURVE('',#3960,#3956,#2432,.T.);
#4795=EDGE_CURVE('',#3961,#3959,#2433,.T.);
#4796=EDGE_CURVE('',#3960,#3961,#2434,.T.);
#4797=EDGE_CURVE('',#3962,#3960,#2435,.T.);
#4798=EDGE_CURVE('',#3963,#3961,#2436,.T.);
#4799=EDGE_CURVE('',#3962,#3963,#2437,.T.);
#4800=EDGE_CURVE('',#3957,#3962,#2438,.T.);
#4801=EDGE_CURVE('',#3958,#3963,#2439,.T.);
#4802=EDGE_CURVE('',#3964,#3965,#2440,.T.);
#4803=EDGE_CURVE('',#3965,#3966,#2441,.T.);
#4804=EDGE_CURVE('',#3967,#3966,#2442,.T.);
#4805=EDGE_CURVE('',#3964,#3967,#2443,.T.);
#4806=EDGE_CURVE('',#3968,#3964,#2444,.T.);
#4807=EDGE_CURVE('',#3969,#3967,#2445,.T.);
#4808=EDGE_CURVE('',#3968,#3969,#2446,.T.);
#4809=EDGE_CURVE('',#3970,#3968,#2447,.T.);
#4810=EDGE_CURVE('',#3971,#3969,#2448,.T.);
#4811=EDGE_CURVE('',#3970,#3971,#2449,.T.);
#4812=EDGE_CURVE('',#3965,#3970,#2450,.T.);
#4813=EDGE_CURVE('',#3966,#3971,#2451,.T.);
#4814=EDGE_CURVE('',#3972,#3973,#2452,.T.);
#4815=EDGE_CURVE('',#3973,#3974,#2453,.T.);
#4816=EDGE_CURVE('',#3975,#3974,#2454,.T.);
#4817=EDGE_CURVE('',#3972,#3975,#2455,.T.);
#4818=EDGE_CURVE('',#3976,#3972,#2456,.T.);
#4819=EDGE_CURVE('',#3977,#3975,#2457,.T.);
#4820=EDGE_CURVE('',#3976,#3977,#2458,.T.);
#4821=EDGE_CURVE('',#3978,#3976,#2459,.T.);
#4822=EDGE_CURVE('',#3979,#3977,#2460,.T.);
#4823=EDGE_CURVE('',#3978,#3979,#2461,.T.);
#4824=EDGE_CURVE('',#3973,#3978,#2462,.T.);
#4825=EDGE_CURVE('',#3974,#3979,#2463,.T.);
#4826=EDGE_CURVE('',#3980,#3980,#3426,.T.);
#4827=EDGE_CURVE('',#3980,#3981,#2464,.T.);
#4828=EDGE_CURVE('',#3981,#3981,#3427,.T.);
#4829=EDGE_CURVE('',#3982,#3982,#3428,.T.);
#4830=EDGE_CURVE('',#3982,#3983,#2465,.T.);
#4831=EDGE_CURVE('',#3983,#3983,#3429,.T.);
#4832=EDGE_CURVE('',#3984,#3985,#2466,.T.);
#4833=EDGE_CURVE('',#3985,#3986,#2467,.T.);
#4834=EDGE_CURVE('',#3987,#3986,#2468,.T.);
#4835=EDGE_CURVE('',#3984,#3987,#2469,.T.);
#4836=EDGE_CURVE('',#3988,#3984,#2470,.T.);
#4837=EDGE_CURVE('',#3989,#3987,#2471,.T.);
#4838=EDGE_CURVE('',#3988,#3989,#2472,.T.);
#4839=EDGE_CURVE('',#3990,#3988,#2473,.T.);
#4840=EDGE_CURVE('',#3991,#3989,#2474,.T.);
#4841=EDGE_CURVE('',#3990,#3991,#2475,.T.);
#4842=EDGE_CURVE('',#3985,#3990,#2476,.T.);
#4843=EDGE_CURVE('',#3986,#3991,#2477,.T.);
#4844=EDGE_CURVE('',#3992,#3993,#2478,.T.);
#4845=EDGE_CURVE('',#3993,#3994,#2479,.T.);
#4846=EDGE_CURVE('',#3995,#3994,#2480,.T.);
#4847=EDGE_CURVE('',#3992,#3995,#2481,.T.);
#4848=EDGE_CURVE('',#3996,#3992,#2482,.T.);
#4849=EDGE_CURVE('',#3997,#3995,#2483,.T.);
#4850=EDGE_CURVE('',#3996,#3997,#2484,.T.);
#4851=EDGE_CURVE('',#3998,#3996,#2485,.T.);
#4852=EDGE_CURVE('',#3999,#3997,#2486,.T.);
#4853=EDGE_CURVE('',#3998,#3999,#2487,.T.);
#4854=EDGE_CURVE('',#3993,#3998,#2488,.T.);
#4855=EDGE_CURVE('',#3994,#3999,#2489,.T.);
#4856=EDGE_CURVE('',#4000,#4001,#2490,.T.);
#4857=EDGE_CURVE('',#4001,#4002,#2491,.T.);
#4858=EDGE_CURVE('',#4003,#4002,#2492,.T.);
#4859=EDGE_CURVE('',#4000,#4003,#2493,.T.);
#4860=EDGE_CURVE('',#4004,#4000,#2494,.T.);
#4861=EDGE_CURVE('',#4005,#4003,#2495,.T.);
#4862=EDGE_CURVE('',#4004,#4005,#2496,.T.);
#4863=EDGE_CURVE('',#4006,#4004,#2497,.T.);
#4864=EDGE_CURVE('',#4007,#4005,#2498,.T.);
#4865=EDGE_CURVE('',#4006,#4007,#2499,.T.);
#4866=EDGE_CURVE('',#4001,#4006,#2500,.T.);
#4867=EDGE_CURVE('',#4002,#4007,#2501,.T.);
#4868=EDGE_CURVE('',#4008,#4008,#3430,.T.);
#4869=EDGE_CURVE('',#4008,#4009,#2502,.T.);
#4870=EDGE_CURVE('',#4009,#4009,#3431,.T.);
#4871=EDGE_CURVE('',#4010,#4010,#3432,.T.);
#4872=EDGE_CURVE('',#4010,#4011,#2503,.T.);
#4873=EDGE_CURVE('',#4011,#4011,#3433,.T.);
#4874=EDGE_CURVE('',#4012,#4012,#3434,.T.);
#4875=EDGE_CURVE('',#4012,#4013,#2504,.T.);
#4876=EDGE_CURVE('',#4013,#4013,#3435,.T.);
#4877=EDGE_CURVE('',#4014,#4014,#3436,.T.);
#4878=EDGE_CURVE('',#4014,#4015,#2505,.T.);
#4879=EDGE_CURVE('',#4015,#4015,#3437,.T.);
#4880=EDGE_CURVE('',#4016,#4016,#3438,.T.);
#4881=EDGE_CURVE('',#4016,#4017,#2506,.T.);
#4882=EDGE_CURVE('',#4017,#4017,#3439,.T.);
#4883=EDGE_CURVE('',#4018,#4018,#3440,.T.);
#4884=EDGE_CURVE('',#4018,#4019,#2507,.T.);
#4885=EDGE_CURVE('',#4019,#4019,#3441,.T.);
#4886=EDGE_CURVE('',#4020,#4020,#3442,.T.);
#4887=EDGE_CURVE('',#4020,#4021,#2508,.T.);
#4888=EDGE_CURVE('',#4021,#4021,#3443,.T.);
#4889=EDGE_CURVE('',#4022,#4022,#3444,.T.);
#4890=EDGE_CURVE('',#4022,#4023,#2509,.T.);
#4891=EDGE_CURVE('',#4023,#4023,#3445,.T.);
#4892=EDGE_CURVE('',#4024,#4024,#3446,.T.);
#4893=EDGE_CURVE('',#4024,#4025,#2510,.T.);
#4894=EDGE_CURVE('',#4025,#4025,#3447,.T.);
#4895=EDGE_CURVE('',#4026,#4026,#3448,.T.);
#4896=EDGE_CURVE('',#4027,#4027,#3449,.T.);
#4897=EDGE_CURVE('',#4027,#4026,#2511,.T.);
#4898=EDGE_CURVE('',#4028,#4028,#3450,.T.);
#4899=EDGE_CURVE('',#4028,#4029,#2512,.T.);
#4900=EDGE_CURVE('',#4029,#4029,#3451,.T.);
#4901=EDGE_CURVE('',#4030,#4030,#3452,.T.);
#4902=EDGE_CURVE('',#4030,#4031,#2513,.T.);
#4903=EDGE_CURVE('',#4031,#4031,#3453,.T.);
#4904=EDGE_CURVE('',#4032,#4032,#3454,.T.);
#4905=EDGE_CURVE('',#4033,#4033,#3455,.T.);
#4906=EDGE_CURVE('',#4033,#4032,#2514,.T.);
#4907=EDGE_CURVE('',#4034,#4034,#3456,.T.);
#4908=EDGE_CURVE('',#4034,#4035,#2515,.T.);
#4909=EDGE_CURVE('',#4035,#4035,#3457,.T.);
#4910=EDGE_CURVE('',#4036,#4036,#3458,.T.);
#4911=EDGE_CURVE('',#4036,#4037,#2516,.T.);
#4912=EDGE_CURVE('',#4037,#4037,#3459,.T.);
#4913=EDGE_CURVE('',#4038,#4038,#3460,.T.);
#4914=EDGE_CURVE('',#4038,#4039,#2517,.T.);
#4915=EDGE_CURVE('',#4039,#4039,#3461,.T.);
#4916=EDGE_CURVE('',#4040,#4040,#3462,.T.);
#4917=EDGE_CURVE('',#4040,#4041,#2518,.T.);
#4918=EDGE_CURVE('',#4041,#4041,#3463,.T.);
#4919=EDGE_CURVE('',#4042,#4042,#3464,.T.);
#4920=EDGE_CURVE('',#4042,#4043,#2519,.T.);
#4921=EDGE_CURVE('',#4043,#4043,#3465,.T.);
#4922=EDGE_CURVE('',#4044,#4044,#3466,.T.);
#4923=EDGE_CURVE('',#4045,#4045,#3467,.T.);
#4924=EDGE_CURVE('',#4045,#4046,#2520,.T.);
#4925=EDGE_CURVE('',#4046,#4046,#3468,.T.);
#4926=EDGE_CURVE('',#4047,#4047,#3469,.T.);
#4927=EDGE_CURVE('',#4048,#4048,#3470,.T.);
#4928=EDGE_CURVE('',#4048,#4044,#2521,.T.);
#4929=EDGE_CURVE('',#4049,#4049,#3471,.T.);
#4930=EDGE_CURVE('',#4049,#4047,#2522,.T.);
#4931=EDGE_CURVE('',#4050,#4050,#3472,.T.);
#4932=EDGE_CURVE('',#4050,#4051,#2523,.T.);
#4933=EDGE_CURVE('',#4051,#4051,#3473,.T.);
#4934=EDGE_CURVE('',#4052,#4053,#2524,.T.);
#4935=EDGE_CURVE('',#4053,#4054,#2525,.T.);
#4936=EDGE_CURVE('',#4055,#4054,#2526,.T.);
#4937=EDGE_CURVE('',#4052,#4055,#2527,.T.);
#4938=EDGE_CURVE('',#4056,#4052,#2528,.T.);
#4939=EDGE_CURVE('',#4057,#4055,#2529,.T.);
#4940=EDGE_CURVE('',#4056,#4057,#2530,.T.);
#4941=EDGE_CURVE('',#4058,#4056,#2531,.T.);
#4942=EDGE_CURVE('',#4059,#4057,#2532,.T.);
#4943=EDGE_CURVE('',#4058,#4059,#2533,.T.);
#4944=EDGE_CURVE('',#4053,#4058,#2534,.T.);
#4945=EDGE_CURVE('',#4054,#4059,#2535,.T.);
#4946=EDGE_CURVE('',#4060,#4060,#3474,.T.);
#4947=EDGE_CURVE('',#4060,#4061,#2536,.T.);
#4948=EDGE_CURVE('',#4061,#4061,#3475,.T.);
#4949=EDGE_CURVE('',#4062,#4062,#3476,.T.);
#4950=EDGE_CURVE('',#4062,#4063,#2537,.T.);
#4951=EDGE_CURVE('',#4063,#4063,#3477,.T.);
#4952=EDGE_CURVE('',#4064,#4064,#3478,.T.);
#4953=EDGE_CURVE('',#4064,#4065,#2538,.T.);
#4954=EDGE_CURVE('',#4065,#4065,#3479,.T.);
#4955=EDGE_CURVE('',#4066,#4066,#3480,.T.);
#4956=EDGE_CURVE('',#4066,#4067,#2539,.T.);
#4957=EDGE_CURVE('',#4067,#4067,#3481,.T.);
#4958=EDGE_CURVE('',#4068,#4069,#3482,.T.);
#4959=EDGE_CURVE('',#4069,#4068,#3483,.T.);
#4960=EDGE_CURVE('',#4069,#4070,#3484,.T.);
#4961=EDGE_CURVE('',#4071,#4070,#3485,.T.);
#4962=EDGE_CURVE('',#4070,#4071,#3486,.T.);
#4963=EDGE_CURVE('',#4071,#4072,#2540,.T.);
#4964=EDGE_CURVE('',#4072,#4072,#3487,.T.);
#4965=EDGE_CURVE('',#4073,#4073,#3488,.T.);
#4966=EDGE_CURVE('',#4073,#4074,#2541,.T.);
#4967=EDGE_CURVE('',#4074,#4074,#3489,.T.);
#4968=EDGE_CURVE('',#4074,#4075,#2542,.T.);
#4969=EDGE_CURVE('',#4075,#4075,#3490,.T.);
#4970=EDGE_CURVE('',#4076,#4076,#3491,.T.);
#4971=EDGE_CURVE('',#4076,#4068,#2543,.T.);
#4972=EDGE_CURVE('',#4077,#4077,#3492,.T.);
#4973=EDGE_CURVE('',#4077,#4073,#2544,.T.);
#4974=EDGE_CURVE('',#4078,#4079,#3493,.T.);
#4975=EDGE_CURVE('',#4079,#4078,#3494,.T.);
#4976=EDGE_CURVE('',#4079,#4080,#3495,.T.);
#4977=EDGE_CURVE('',#4081,#4080,#3496,.T.);
#4978=EDGE_CURVE('',#4080,#4081,#3497,.T.);
#4979=EDGE_CURVE('',#4082,#4082,#3498,.T.);
#4980=EDGE_CURVE('',#4082,#4081,#2545,.T.);
#4981=EDGE_CURVE('',#4083,#4083,#3499,.T.);
#4982=EDGE_CURVE('',#4084,#4084,#3500,.T.);
#4983=EDGE_CURVE('',#4085,#4085,#3501,.T.);
#4984=EDGE_CURVE('',#4085,#4083,#2546,.T.);
#4985=EDGE_CURVE('',#4086,#4086,#3502,.T.);
#4986=EDGE_CURVE('',#4086,#4085,#2547,.T.);
#4987=EDGE_CURVE('',#4087,#4087,#3503,.T.);
#4988=EDGE_CURVE('',#4087,#4086,#2548,.T.);
#4989=EDGE_CURVE('',#4078,#4084,#2549,.T.);
#4990=EDGE_CURVE('',#4088,#4089,#3504,.T.);
#4991=EDGE_CURVE('',#4090,#4091,#3505,.T.);
#4992=EDGE_CURVE('',#4092,#4093,#3506,.T.);
#4993=EDGE_CURVE('',#4094,#4095,#3507,.T.);
#4994=EDGE_CURVE('',#4096,#4097,#3508,.T.);
#4995=EDGE_CURVE('',#4098,#4099,#3509,.T.);
#4996=EDGE_CURVE('',#4100,#4101,#3510,.T.);
#4997=EDGE_CURVE('',#4102,#4103,#3511,.T.);
#4998=EDGE_CURVE('',#4104,#4105,#443,.T.);
#4999=EDGE_CURVE('',#4106,#4104,#3512,.T.);
#5000=EDGE_CURVE('',#4107,#4106,#444,.T.);
#5001=EDGE_CURVE('',#4105,#4107,#3513,.T.);
#5002=EDGE_CURVE('',#4108,#4106,#3514,.T.);
#5003=EDGE_CURVE('',#4108,#4109,#445,.T.);
#5004=EDGE_CURVE('',#4110,#4109,#3515,.T.);
#5005=EDGE_CURVE('',#4110,#4111,#446,.T.);
#5006=EDGE_CURVE('',#4112,#4111,#3516,.T.);
#5007=EDGE_CURVE('',#4112,#4113,#447,.T.);
#5008=EDGE_CURVE('',#4113,#4114,#2550,.T.);
#5009=EDGE_CURVE('',#4114,#4114,#3517,.T.);
#5010=EDGE_CURVE('',#4113,#4115,#448,.T.);
#5011=EDGE_CURVE('',#4116,#4115,#3518,.T.);
#5012=EDGE_CURVE('',#4116,#4117,#449,.T.);
#5013=EDGE_CURVE('',#4118,#4117,#3519,.T.);
#5014=EDGE_CURVE('',#4118,#4119,#450,.T.);
#5015=EDGE_CURVE('',#4120,#4119,#3520,.T.);
#5016=EDGE_CURVE('',#4120,#4121,#451,.T.);
#5017=EDGE_CURVE('',#4122,#4121,#3521,.T.);
#5018=EDGE_CURVE('',#4122,#4123,#452,.T.);
#5019=EDGE_CURVE('',#4107,#4123,#3522,.T.);
#5020=EDGE_CURVE('',#4104,#4124,#3523,.T.);
#5021=EDGE_CURVE('',#4124,#4108,#3524,.T.);
#5022=EDGE_CURVE('',#4125,#4124,#453,.T.);
#5023=EDGE_CURVE('',#4109,#4125,#3525,.T.);
#5024=EDGE_CURVE('',#4125,#4126,#3526,.T.);
#5025=EDGE_CURVE('',#4126,#4110,#3527,.T.);
#5026=EDGE_CURVE('',#4127,#4126,#454,.T.);
#5027=EDGE_CURVE('',#4111,#4127,#3528,.T.);
#5028=EDGE_CURVE('',#4127,#4128,#3529,.T.);
#5029=EDGE_CURVE('',#4128,#4112,#3530,.T.);
#5030=EDGE_CURVE('',#4129,#4130,#455,.T.);
#5031=EDGE_CURVE('',#4115,#4129,#3531,.T.);
#5032=EDGE_CURVE('',#4130,#4128,#456,.T.);
#5033=EDGE_CURVE('',#4129,#4131,#3532,.T.);
#5034=EDGE_CURVE('',#4131,#4116,#3533,.T.);
#5035=EDGE_CURVE('',#4132,#4131,#457,.T.);
#5036=EDGE_CURVE('',#4117,#4132,#3534,.T.);
#5037=EDGE_CURVE('',#4132,#4133,#3535,.T.);
#5038=EDGE_CURVE('',#4133,#4118,#3536,.T.);
#5039=EDGE_CURVE('',#4134,#4133,#458,.T.);
#5040=EDGE_CURVE('',#4119,#4134,#3537,.T.);
#5041=EDGE_CURVE('',#4134,#4135,#3538,.T.);
#5042=EDGE_CURVE('',#4135,#4120,#3539,.T.);
#5043=EDGE_CURVE('',#4136,#4135,#459,.T.);
#5044=EDGE_CURVE('',#4121,#4136,#3540,.T.);
#5045=EDGE_CURVE('',#4137,#4137,#3541,.T.);
#5046=EDGE_CURVE('',#4137,#4130,#2551,.T.);
#5047=EDGE_CURVE('',#4138,#4105,#3542,.T.);
#5048=EDGE_CURVE('',#4138,#4139,#460,.T.);
#5049=EDGE_CURVE('',#4136,#4139,#3543,.T.);
#5050=EDGE_CURVE('',#4123,#4138,#3544,.T.);
#5051=EDGE_CURVE('',#4139,#4122,#3545,.T.);
#5052=EDGE_CURVE('',#4140,#4140,#3546,.T.);
#5053=EDGE_CURVE('',#4141,#4141,#3547,.T.);
#5054=EDGE_CURVE('',#4142,#4142,#3548,.T.);
#5055=EDGE_CURVE('',#4142,#4140,#2552,.T.);
#5056=EDGE_CURVE('',#4143,#4143,#3549,.T.);
#5057=EDGE_CURVE('',#4143,#4141,#2553,.T.);
#5058=EDGE_CURVE('',#4144,#4144,#3550,.T.);
#5059=EDGE_CURVE('',#4145,#4145,#3551,.T.);
#5060=EDGE_CURVE('',#4146,#4146,#3552,.T.);
#5061=EDGE_CURVE('',#4146,#4144,#2554,.T.);
#5062=EDGE_CURVE('',#4147,#4147,#3553,.T.);
#5063=EDGE_CURVE('',#4147,#4145,#2555,.T.);
#5064=EDGE_CURVE('',#4148,#4148,#3554,.T.);
#5065=EDGE_CURVE('',#4148,#4149,#2556,.T.);
#5066=EDGE_CURVE('',#4149,#4149,#3555,.T.);
#5067=EDGE_CURVE('',#4150,#4150,#3556,.T.);
#5068=EDGE_CURVE('',#4150,#4151,#2557,.T.);
#5069=EDGE_CURVE('',#4151,#4151,#3557,.T.);
#5070=EDGE_CURVE('',#4152,#4153,#2558,.T.);
#5071=EDGE_CURVE('',#4153,#4154,#2559,.T.);
#5072=EDGE_CURVE('',#4154,#4155,#2560,.T.);
#5073=EDGE_CURVE('',#4152,#4155,#2561,.T.);
#5074=EDGE_CURVE('',#4153,#4156,#2562,.T.);
#5075=EDGE_CURVE('',#4156,#4157,#2563,.T.);
#5076=EDGE_CURVE('',#4157,#4154,#2564,.T.);
#5077=EDGE_CURVE('',#4156,#4158,#2565,.T.);
#5078=EDGE_CURVE('',#4158,#4159,#2566,.T.);
#5079=EDGE_CURVE('',#4159,#4157,#2567,.T.);
#5080=EDGE_CURVE('',#4158,#4160,#2568,.T.);
#5081=EDGE_CURVE('',#4160,#4161,#2569,.T.);
#5082=EDGE_CURVE('',#4161,#4159,#2570,.T.);
#5083=EDGE_CURVE('',#4160,#4162,#2571,.T.);
#5084=EDGE_CURVE('',#4162,#4163,#2572,.T.);
#5085=EDGE_CURVE('',#4163,#4161,#2573,.T.);
#5086=EDGE_CURVE('',#4162,#4152,#2574,.T.);
#5087=EDGE_CURVE('',#4155,#4163,#2575,.T.);
#5088=EDGE_CURVE('',#4164,#4164,#3558,.T.);
#5089=EDGE_CURVE('',#4165,#4165,#3559,.T.);
#5090=EDGE_CURVE('',#4166,#4166,#3560,.T.);
#5091=EDGE_CURVE('',#4166,#4165,#2576,.T.);
#5092=EDGE_CURVE('',#4167,#4167,#3561,.T.);
#5093=EDGE_CURVE('',#4167,#4166,#2577,.T.);
#5094=EDGE_CURVE('',#4168,#4168,#3562,.T.);
#5095=EDGE_CURVE('',#4168,#4167,#2578,.T.);
#5096=EDGE_CURVE('',#4169,#4169,#3563,.T.);
#5097=EDGE_CURVE('',#4170,#4170,#3564,.F.);
#5098=EDGE_CURVE('',#4170,#4169,#2579,.T.);
#5099=EDGE_CURVE('',#4164,#4170,#2580,.T.);
#5100=EDGE_CURVE('',#4171,#4171,#3565,.T.);
#5101=EDGE_CURVE('',#4171,#4172,#2581,.T.);
#5102=EDGE_CURVE('',#4172,#4172,#3566,.T.);
#5103=EDGE_CURVE('',#4173,#4173,#3567,.T.);
#5104=EDGE_CURVE('',#4173,#4174,#2582,.T.);
#5105=EDGE_CURVE('',#4174,#4174,#3568,.T.);
#5106=EDGE_CURVE('',#4175,#4176,#2583,.T.);
#5107=EDGE_CURVE('',#4177,#4175,#2584,.T.);
#5108=EDGE_CURVE('',#4178,#4177,#2585,.T.);
#5109=EDGE_CURVE('',#4176,#4178,#2586,.T.);
#5110=EDGE_CURVE('',#4177,#4179,#2587,.T.);
#5111=EDGE_CURVE('',#4180,#4179,#2588,.T.);
#5112=EDGE_CURVE('',#4178,#4180,#2589,.T.);
#5113=EDGE_CURVE('',#4179,#4181,#2590,.T.);
#5114=EDGE_CURVE('',#4181,#4182,#2591,.T.);
#5115=EDGE_CURVE('',#4182,#4180,#2592,.T.);
#5116=EDGE_CURVE('',#4183,#4183,#3569,.T.);
#5117=EDGE_CURVE('',#4184,#4175,#2593,.T.);
#5118=EDGE_CURVE('',#4185,#4184,#2594,.T.);
#5119=EDGE_CURVE('',#4185,#4186,#2595,.T.);
#5120=EDGE_CURVE('',#4187,#4186,#2596,.T.);
#5121=EDGE_CURVE('',#4187,#4188,#2597,.T.);
#5122=EDGE_CURVE('',#4188,#4189,#2598,.T.);
#5123=EDGE_CURVE('',#4189,#4181,#2599,.T.);
#5124=EDGE_CURVE('',#4189,#4190,#2600,.T.);
#5125=EDGE_CURVE('',#4190,#4182,#2601,.T.);
#5126=EDGE_CURVE('',#4191,#4188,#2602,.T.);
#5127=EDGE_CURVE('',#4190,#4191,#2603,.T.);
#5128=EDGE_CURVE('',#4192,#4191,#2604,.T.);
#5129=EDGE_CURVE('',#4193,#4192,#2605,.T.);
#5130=EDGE_CURVE('',#4193,#4194,#2606,.T.);
#5131=EDGE_CURVE('',#4195,#4194,#2607,.T.);
#5132=EDGE_CURVE('',#4195,#4176,#2608,.T.);
#5133=EDGE_CURVE('',#4192,#4187,#2609,.T.);
#5134=EDGE_CURVE('',#4186,#4196,#2610,.T.);
#5135=EDGE_CURVE('',#4196,#4197,#11,.T.);
#5136=EDGE_CURVE('',#4197,#4193,#2611,.T.);
#5137=EDGE_CURVE('',#4198,#4196,#3570,.F.);
#5138=EDGE_CURVE('',#4198,#4183,#2612,.T.);
#5139=EDGE_CURVE('',#4199,#4198,#3571,.F.);
#5140=EDGE_CURVE('',#4200,#4199,#12,.T.);
#5141=EDGE_CURVE('',#4197,#4200,#3572,.F.);
#5142=EDGE_CURVE('',#4199,#4185,#2613,.T.);
#5143=EDGE_CURVE('',#4194,#4200,#2614,.T.);
#5144=EDGE_CURVE('',#4184,#4195,#2615,.T.);
#5145=EDGE_CURVE('',#4201,#4202,#2616,.T.);
#5146=EDGE_CURVE('',#4202,#4203,#2617,.T.);
#5147=EDGE_CURVE('',#4203,#4204,#2618,.T.);
#5148=EDGE_CURVE('',#4201,#4204,#2619,.T.);
#5149=EDGE_CURVE('',#4202,#4205,#2620,.T.);
#5150=EDGE_CURVE('',#4205,#4206,#2621,.T.);
#5151=EDGE_CURVE('',#4206,#4203,#2622,.T.);
#5152=EDGE_CURVE('',#4205,#4207,#2623,.T.);
#5153=EDGE_CURVE('',#4207,#4208,#2624,.T.);
#5154=EDGE_CURVE('',#4208,#4206,#2625,.T.);
#5155=EDGE_CURVE('',#4207,#4209,#2626,.T.);
#5156=EDGE_CURVE('',#4209,#4210,#2627,.T.);
#5157=EDGE_CURVE('',#4210,#4208,#2628,.T.);
#5158=EDGE_CURVE('',#4209,#4211,#2629,.T.);
#5159=EDGE_CURVE('',#4211,#4212,#2630,.T.);
#5160=EDGE_CURVE('',#4212,#4210,#2631,.T.);
#5161=EDGE_CURVE('',#4211,#4201,#2632,.T.);
#5162=EDGE_CURVE('',#4204,#4212,#2633,.T.);
#5163=EDGE_CURVE('',#4213,#4213,#3573,.T.);
#5164=EDGE_CURVE('',#4214,#4214,#3574,.T.);
#5165=EDGE_CURVE('',#4215,#4215,#3575,.T.);
#5166=EDGE_CURVE('',#4215,#4214,#2634,.T.);
#5167=EDGE_CURVE('',#4216,#4216,#3576,.T.);
#5168=EDGE_CURVE('',#4216,#4215,#2635,.T.);
#5169=EDGE_CURVE('',#4217,#4217,#3577,.T.);
#5170=EDGE_CURVE('',#4217,#4216,#2636,.T.);
#5171=EDGE_CURVE('',#4218,#4218,#3578,.T.);
#5172=EDGE_CURVE('',#4219,#4219,#3579,.F.);
#5173=EDGE_CURVE('',#4219,#4218,#2637,.T.);
#5174=EDGE_CURVE('',#4213,#4219,#2638,.T.);
#5175=EDGE_CURVE('',#4220,#4220,#3580,.T.);
#5176=EDGE_CURVE('',#4220,#4221,#2639,.T.);
#5177=EDGE_CURVE('',#4221,#4221,#3581,.T.);
#5178=EDGE_CURVE('',#4222,#4222,#3582,.T.);
#5179=EDGE_CURVE('',#4223,#4223,#3583,.T.);
#5180=EDGE_CURVE('',#4223,#4224,#2640,.T.);
#5181=EDGE_CURVE('',#4224,#4224,#3584,.T.);
#5182=EDGE_CURVE('',#4225,#4225,#3585,.T.);
#5183=EDGE_CURVE('',#4226,#4226,#3586,.T.);
#5184=EDGE_CURVE('',#4226,#4222,#2641,.T.);
#5185=EDGE_CURVE('',#4227,#4227,#3587,.T.);
#5186=EDGE_CURVE('',#4227,#4225,#2642,.T.);
#5187=EDGE_CURVE('',#4228,#4228,#3588,.T.);
#5188=EDGE_CURVE('',#4228,#4229,#2643,.T.);
#5189=EDGE_CURVE('',#4229,#4229,#3589,.T.);
#5190=EDGE_CURVE('',#4230,#4231,#2644,.T.);
#5191=EDGE_CURVE('',#4231,#4232,#2645,.T.);
#5192=EDGE_CURVE('',#4233,#4232,#2646,.T.);
#5193=EDGE_CURVE('',#4230,#4233,#2647,.T.);
#5194=EDGE_CURVE('',#4234,#4230,#2648,.T.);
#5195=EDGE_CURVE('',#4235,#4233,#2649,.T.);
#5196=EDGE_CURVE('',#4234,#4235,#2650,.T.);
#5197=EDGE_CURVE('',#4236,#4234,#2651,.T.);
#5198=EDGE_CURVE('',#4237,#4235,#2652,.T.);
#5199=EDGE_CURVE('',#4236,#4237,#2653,.T.);
#5200=EDGE_CURVE('',#4231,#4236,#2654,.T.);
#5201=EDGE_CURVE('',#4232,#4237,#2655,.T.);
#5202=ORIENTED_EDGE('',*,*,#4238,.F.);
#5203=ORIENTED_EDGE('',*,*,#4239,.T.);
#5204=ORIENTED_EDGE('',*,*,#4240,.F.);
#5205=ORIENTED_EDGE('',*,*,#4239,.F.);
#5206=ORIENTED_EDGE('',*,*,#4241,.F.);
#5207=ORIENTED_EDGE('',*,*,#4242,.T.);
#5208=ORIENTED_EDGE('',*,*,#4243,.F.);
#5209=ORIENTED_EDGE('',*,*,#4242,.F.);
#5210=ORIENTED_EDGE('',*,*,#4244,.F.);
#5211=ORIENTED_EDGE('',*,*,#4245,.T.);
#5212=ORIENTED_EDGE('',*,*,#4246,.F.);
#5213=ORIENTED_EDGE('',*,*,#4245,.F.);
#5214=ORIENTED_EDGE('',*,*,#4247,.F.);
#5215=ORIENTED_EDGE('',*,*,#4248,.T.);
#5216=ORIENTED_EDGE('',*,*,#4249,.F.);
#5217=ORIENTED_EDGE('',*,*,#4248,.F.);
#5218=ORIENTED_EDGE('',*,*,#4250,.T.);
#5219=ORIENTED_EDGE('',*,*,#4251,.T.);
#5220=ORIENTED_EDGE('',*,*,#4252,.F.);
#5221=ORIENTED_EDGE('',*,*,#4253,.F.);
#5222=ORIENTED_EDGE('',*,*,#4240,.T.);
#5223=ORIENTED_EDGE('',*,*,#4243,.T.);
#5224=ORIENTED_EDGE('',*,*,#4246,.T.);
#5225=ORIENTED_EDGE('',*,*,#4249,.T.);
#5226=ORIENTED_EDGE('',*,*,#4254,.T.);
#5227=ORIENTED_EDGE('',*,*,#4253,.T.);
#5228=ORIENTED_EDGE('',*,*,#4255,.F.);
#5229=ORIENTED_EDGE('',*,*,#4256,.F.);
#5230=ORIENTED_EDGE('',*,*,#4257,.T.);
#5231=ORIENTED_EDGE('',*,*,#4256,.T.);
#5232=ORIENTED_EDGE('',*,*,#4258,.F.);
#5233=ORIENTED_EDGE('',*,*,#4259,.F.);
#5234=ORIENTED_EDGE('',*,*,#4238,.T.);
#5235=ORIENTED_EDGE('',*,*,#4241,.T.);
#5236=ORIENTED_EDGE('',*,*,#4244,.T.);
#5237=ORIENTED_EDGE('',*,*,#4247,.T.);
#5238=ORIENTED_EDGE('',*,*,#4260,.T.);
#5239=ORIENTED_EDGE('',*,*,#4259,.T.);
#5240=ORIENTED_EDGE('',*,*,#4261,.F.);
#5241=ORIENTED_EDGE('',*,*,#4251,.F.);
#5242=ORIENTED_EDGE('',*,*,#4261,.T.);
#5243=ORIENTED_EDGE('',*,*,#4258,.T.);
#5244=ORIENTED_EDGE('',*,*,#4255,.T.);
#5245=ORIENTED_EDGE('',*,*,#4252,.T.);
#5246=ORIENTED_EDGE('',*,*,#4260,.F.);
#5247=ORIENTED_EDGE('',*,*,#4250,.F.);
#5248=ORIENTED_EDGE('',*,*,#4254,.F.);
#5249=ORIENTED_EDGE('',*,*,#4257,.F.);
#5250=ORIENTED_EDGE('',*,*,#4262,.F.);
#5251=ORIENTED_EDGE('',*,*,#4263,.T.);
#5252=ORIENTED_EDGE('',*,*,#4264,.F.);
#5253=ORIENTED_EDGE('',*,*,#4265,.T.);
#5254=ORIENTED_EDGE('',*,*,#4266,.F.);
#5255=ORIENTED_EDGE('',*,*,#4265,.F.);
#5256=ORIENTED_EDGE('',*,*,#4267,.F.);
#5257=ORIENTED_EDGE('',*,*,#4268,.F.);
#5258=ORIENTED_EDGE('',*,*,#4263,.F.);
#5259=ORIENTED_EDGE('',*,*,#4269,.F.);
#5260=ORIENTED_EDGE('',*,*,#4270,.F.);
#5261=ORIENTED_EDGE('',*,*,#4271,.F.);
#5262=ORIENTED_EDGE('',*,*,#4272,.T.);
#5263=ORIENTED_EDGE('',*,*,#4264,.T.);
#5264=ORIENTED_EDGE('',*,*,#4268,.T.);
#5265=ORIENTED_EDGE('',*,*,#4267,.T.);
#5266=ORIENTED_EDGE('',*,*,#4272,.F.);
#5267=ORIENTED_EDGE('',*,*,#4273,.F.);
#5268=ORIENTED_EDGE('',*,*,#4274,.T.);
#5269=ORIENTED_EDGE('',*,*,#4275,.F.);
#5270=ORIENTED_EDGE('',*,*,#4276,.F.);
#5271=ORIENTED_EDGE('',*,*,#4277,.F.);
#5272=ORIENTED_EDGE('',*,*,#4278,.T.);
#5273=ORIENTED_EDGE('',*,*,#4279,.F.);
#5274=ORIENTED_EDGE('',*,*,#4274,.F.);
#5275=ORIENTED_EDGE('',*,*,#4280,.F.);
#5276=ORIENTED_EDGE('',*,*,#4281,.T.);
#5277=ORIENTED_EDGE('',*,*,#4282,.F.);
#5278=ORIENTED_EDGE('',*,*,#4278,.F.);
#5279=ORIENTED_EDGE('',*,*,#4283,.F.);
#5280=ORIENTED_EDGE('',*,*,#4284,.T.);
#5281=ORIENTED_EDGE('',*,*,#4285,.F.);
#5282=ORIENTED_EDGE('',*,*,#4281,.F.);
#5283=ORIENTED_EDGE('',*,*,#4286,.F.);
#5284=ORIENTED_EDGE('',*,*,#4287,.T.);
#5285=ORIENTED_EDGE('',*,*,#4288,.F.);
#5286=ORIENTED_EDGE('',*,*,#4284,.F.);
#5287=ORIENTED_EDGE('',*,*,#4289,.F.);
#5288=ORIENTED_EDGE('',*,*,#4290,.T.);
#5289=ORIENTED_EDGE('',*,*,#4291,.F.);
#5290=ORIENTED_EDGE('',*,*,#4287,.F.);
#5291=ORIENTED_EDGE('',*,*,#4292,.F.);
#5292=ORIENTED_EDGE('',*,*,#4293,.T.);
#5293=ORIENTED_EDGE('',*,*,#4294,.F.);
#5294=ORIENTED_EDGE('',*,*,#4290,.F.);
#5295=ORIENTED_EDGE('',*,*,#4295,.F.);
#5296=ORIENTED_EDGE('',*,*,#4296,.T.);
#5297=ORIENTED_EDGE('',*,*,#4297,.F.);
#5298=ORIENTED_EDGE('',*,*,#4293,.F.);
#5299=ORIENTED_EDGE('',*,*,#4298,.F.);
#5300=ORIENTED_EDGE('',*,*,#4299,.F.);
#5301=ORIENTED_EDGE('',*,*,#4300,.F.);
#5302=ORIENTED_EDGE('',*,*,#4296,.F.);
#5303=ORIENTED_EDGE('',*,*,#4301,.F.);
#5304=ORIENTED_EDGE('',*,*,#4302,.T.);
#5305=ORIENTED_EDGE('',*,*,#4303,.F.);
#5306=ORIENTED_EDGE('',*,*,#4304,.F.);
#5307=ORIENTED_EDGE('',*,*,#4305,.F.);
#5308=ORIENTED_EDGE('',*,*,#4306,.T.);
#5309=ORIENTED_EDGE('',*,*,#4307,.F.);
#5310=ORIENTED_EDGE('',*,*,#4302,.F.);
#5311=ORIENTED_EDGE('',*,*,#4308,.F.);
#5312=ORIENTED_EDGE('',*,*,#4309,.T.);
#5313=ORIENTED_EDGE('',*,*,#4310,.F.);
#5314=ORIENTED_EDGE('',*,*,#4306,.F.);
#5315=ORIENTED_EDGE('',*,*,#4311,.F.);
#5316=ORIENTED_EDGE('',*,*,#4312,.T.);
#5317=ORIENTED_EDGE('',*,*,#4313,.F.);
#5318=ORIENTED_EDGE('',*,*,#4309,.F.);
#5319=ORIENTED_EDGE('',*,*,#4314,.F.);
#5320=ORIENTED_EDGE('',*,*,#4315,.T.);
#5321=ORIENTED_EDGE('',*,*,#4316,.F.);
#5322=ORIENTED_EDGE('',*,*,#4312,.F.);
#5323=ORIENTED_EDGE('',*,*,#4262,.T.);
#5324=ORIENTED_EDGE('',*,*,#4317,.F.);
#5325=ORIENTED_EDGE('',*,*,#4318,.T.);
#5326=ORIENTED_EDGE('',*,*,#4319,.F.);
#5327=ORIENTED_EDGE('',*,*,#4315,.F.);
#5328=ORIENTED_EDGE('',*,*,#4320,.F.);
#5329=ORIENTED_EDGE('',*,*,#4321,.T.);
#5330=ORIENTED_EDGE('',*,*,#4322,.F.);
#5331=ORIENTED_EDGE('',*,*,#4318,.F.);
#5332=ORIENTED_EDGE('',*,*,#4323,.F.);
#5333=ORIENTED_EDGE('',*,*,#4324,.T.);
#5334=ORIENTED_EDGE('',*,*,#4325,.F.);
#5335=ORIENTED_EDGE('',*,*,#4321,.F.);
#5336=ORIENTED_EDGE('',*,*,#4326,.F.);
#5337=ORIENTED_EDGE('',*,*,#4327,.F.);
#5338=ORIENTED_EDGE('',*,*,#4328,.F.);
#5339=ORIENTED_EDGE('',*,*,#4324,.F.);
#5340=ORIENTED_EDGE('',*,*,#4329,.F.);
#5341=ORIENTED_EDGE('',*,*,#4330,.T.);
#5342=ORIENTED_EDGE('',*,*,#4331,.F.);
#5343=ORIENTED_EDGE('',*,*,#4332,.F.);
#5344=ORIENTED_EDGE('',*,*,#4333,.F.);
#5345=ORIENTED_EDGE('',*,*,#4334,.T.);
#5346=ORIENTED_EDGE('',*,*,#4335,.F.);
#5347=ORIENTED_EDGE('',*,*,#4330,.F.);
#5348=ORIENTED_EDGE('',*,*,#4336,.F.);
#5349=ORIENTED_EDGE('',*,*,#4337,.T.);
#5350=ORIENTED_EDGE('',*,*,#4338,.F.);
#5351=ORIENTED_EDGE('',*,*,#4334,.F.);
#5352=ORIENTED_EDGE('',*,*,#4339,.F.);
#5353=ORIENTED_EDGE('',*,*,#4340,.T.);
#5354=ORIENTED_EDGE('',*,*,#4341,.F.);
#5355=ORIENTED_EDGE('',*,*,#4337,.F.);
#5356=ORIENTED_EDGE('',*,*,#4342,.F.);
#5357=ORIENTED_EDGE('',*,*,#4343,.T.);
#5358=ORIENTED_EDGE('',*,*,#4344,.F.);
#5359=ORIENTED_EDGE('',*,*,#4340,.F.);
#5360=ORIENTED_EDGE('',*,*,#4345,.F.);
#5361=ORIENTED_EDGE('',*,*,#4346,.T.);
#5362=ORIENTED_EDGE('',*,*,#4347,.F.);
#5363=ORIENTED_EDGE('',*,*,#4343,.F.);
#5364=ORIENTED_EDGE('',*,*,#4348,.F.);
#5365=ORIENTED_EDGE('',*,*,#4349,.T.);
#5366=ORIENTED_EDGE('',*,*,#4350,.F.);
#5367=ORIENTED_EDGE('',*,*,#4346,.F.);
#5368=ORIENTED_EDGE('',*,*,#4351,.F.);
#5369=ORIENTED_EDGE('',*,*,#4352,.T.);
#5370=ORIENTED_EDGE('',*,*,#4353,.F.);
#5371=ORIENTED_EDGE('',*,*,#4349,.F.);
#5372=ORIENTED_EDGE('',*,*,#4354,.F.);
#5373=ORIENTED_EDGE('',*,*,#4355,.F.);
#5374=ORIENTED_EDGE('',*,*,#4356,.F.);
#5375=ORIENTED_EDGE('',*,*,#4352,.F.);
#5376=ORIENTED_EDGE('',*,*,#4357,.F.);
#5377=ORIENTED_EDGE('',*,*,#4358,.T.);
#5378=ORIENTED_EDGE('',*,*,#4359,.F.);
#5379=ORIENTED_EDGE('',*,*,#4360,.F.);
#5380=ORIENTED_EDGE('',*,*,#4361,.F.);
#5381=ORIENTED_EDGE('',*,*,#4362,.T.);
#5382=ORIENTED_EDGE('',*,*,#4363,.F.);
#5383=ORIENTED_EDGE('',*,*,#4358,.F.);
#5384=ORIENTED_EDGE('',*,*,#4364,.F.);
#5385=ORIENTED_EDGE('',*,*,#4365,.T.);
#5386=ORIENTED_EDGE('',*,*,#4366,.F.);
#5387=ORIENTED_EDGE('',*,*,#4362,.F.);
#5388=ORIENTED_EDGE('',*,*,#4367,.F.);
#5389=ORIENTED_EDGE('',*,*,#4368,.T.);
#5390=ORIENTED_EDGE('',*,*,#4369,.F.);
#5391=ORIENTED_EDGE('',*,*,#4365,.F.);
#5392=ORIENTED_EDGE('',*,*,#4370,.F.);
#5393=ORIENTED_EDGE('',*,*,#4371,.T.);
#5394=ORIENTED_EDGE('',*,*,#4372,.F.);
#5395=ORIENTED_EDGE('',*,*,#4368,.F.);
#5396=ORIENTED_EDGE('',*,*,#4266,.T.);
#5397=ORIENTED_EDGE('',*,*,#4373,.F.);
#5398=ORIENTED_EDGE('',*,*,#4374,.T.);
#5399=ORIENTED_EDGE('',*,*,#4375,.F.);
#5400=ORIENTED_EDGE('',*,*,#4371,.F.);
#5401=ORIENTED_EDGE('',*,*,#4376,.F.);
#5402=ORIENTED_EDGE('',*,*,#4377,.T.);
#5403=ORIENTED_EDGE('',*,*,#4378,.F.);
#5404=ORIENTED_EDGE('',*,*,#4374,.F.);
#5405=ORIENTED_EDGE('',*,*,#4379,.F.);
#5406=ORIENTED_EDGE('',*,*,#4380,.T.);
#5407=ORIENTED_EDGE('',*,*,#4381,.F.);
#5408=ORIENTED_EDGE('',*,*,#4377,.F.);
#5409=ORIENTED_EDGE('',*,*,#4382,.F.);
#5410=ORIENTED_EDGE('',*,*,#4383,.F.);
#5411=ORIENTED_EDGE('',*,*,#4384,.F.);
#5412=ORIENTED_EDGE('',*,*,#4380,.F.);
#5413=ORIENTED_EDGE('',*,*,#4269,.T.);
#5414=ORIENTED_EDGE('',*,*,#4385,.T.);
#5415=ORIENTED_EDGE('',*,*,#4386,.F.);
#5416=ORIENTED_EDGE('',*,*,#4385,.F.);
#5417=ORIENTED_EDGE('',*,*,#4270,.T.);
#5418=ORIENTED_EDGE('',*,*,#4299,.T.);
#5419=ORIENTED_EDGE('',*,*,#4387,.T.);
#5420=ORIENTED_EDGE('',*,*,#4388,.T.);
#5421=ORIENTED_EDGE('',*,*,#4389,.F.);
#5422=ORIENTED_EDGE('',*,*,#4276,.T.);
#5423=ORIENTED_EDGE('',*,*,#4390,.F.);
#5424=ORIENTED_EDGE('',*,*,#4391,.F.);
#5425=ORIENTED_EDGE('',*,*,#4392,.T.);
#5426=ORIENTED_EDGE('',*,*,#4327,.T.);
#5427=ORIENTED_EDGE('',*,*,#4393,.T.);
#5428=ORIENTED_EDGE('',*,*,#4391,.T.);
#5429=ORIENTED_EDGE('',*,*,#4394,.F.);
#5430=ORIENTED_EDGE('',*,*,#4304,.T.);
#5431=ORIENTED_EDGE('',*,*,#4395,.F.);
#5432=ORIENTED_EDGE('',*,*,#4396,.F.);
#5433=ORIENTED_EDGE('',*,*,#4397,.T.);
#5434=ORIENTED_EDGE('',*,*,#4355,.T.);
#5435=ORIENTED_EDGE('',*,*,#4398,.T.);
#5436=ORIENTED_EDGE('',*,*,#4396,.T.);
#5437=ORIENTED_EDGE('',*,*,#4399,.F.);
#5438=ORIENTED_EDGE('',*,*,#4332,.T.);
#5439=ORIENTED_EDGE('',*,*,#4400,.F.);
#5440=ORIENTED_EDGE('',*,*,#4401,.F.);
#5441=ORIENTED_EDGE('',*,*,#4402,.T.);
#5442=ORIENTED_EDGE('',*,*,#4383,.T.);
#5443=ORIENTED_EDGE('',*,*,#4403,.T.);
#5444=ORIENTED_EDGE('',*,*,#4401,.T.);
#5445=ORIENTED_EDGE('',*,*,#4404,.F.);
#5446=ORIENTED_EDGE('',*,*,#4360,.T.);
#5447=ORIENTED_EDGE('',*,*,#4405,.F.);
#5448=ORIENTED_EDGE('',*,*,#4388,.F.);
#5449=ORIENTED_EDGE('',*,*,#4406,.T.);
#5450=ORIENTED_EDGE('',*,*,#4275,.T.);
#5451=ORIENTED_EDGE('',*,*,#4279,.T.);
#5452=ORIENTED_EDGE('',*,*,#4282,.T.);
#5453=ORIENTED_EDGE('',*,*,#4285,.T.);
#5454=ORIENTED_EDGE('',*,*,#4288,.T.);
#5455=ORIENTED_EDGE('',*,*,#4291,.T.);
#5456=ORIENTED_EDGE('',*,*,#4294,.T.);
#5457=ORIENTED_EDGE('',*,*,#4297,.T.);
#5458=ORIENTED_EDGE('',*,*,#4300,.T.);
#5459=ORIENTED_EDGE('',*,*,#4389,.T.);
#5460=ORIENTED_EDGE('',*,*,#4405,.T.);
#5461=ORIENTED_EDGE('',*,*,#4359,.T.);
#5462=ORIENTED_EDGE('',*,*,#4363,.T.);
#5463=ORIENTED_EDGE('',*,*,#4366,.T.);
#5464=ORIENTED_EDGE('',*,*,#4369,.T.);
#5465=ORIENTED_EDGE('',*,*,#4372,.T.);
#5466=ORIENTED_EDGE('',*,*,#4375,.T.);
#5467=ORIENTED_EDGE('',*,*,#4378,.T.);
#5468=ORIENTED_EDGE('',*,*,#4381,.T.);
#5469=ORIENTED_EDGE('',*,*,#4384,.T.);
#5470=ORIENTED_EDGE('',*,*,#4404,.T.);
#5471=ORIENTED_EDGE('',*,*,#4400,.T.);
#5472=ORIENTED_EDGE('',*,*,#4331,.T.);
#5473=ORIENTED_EDGE('',*,*,#4335,.T.);
#5474=ORIENTED_EDGE('',*,*,#4338,.T.);
#5475=ORIENTED_EDGE('',*,*,#4341,.T.);
#5476=ORIENTED_EDGE('',*,*,#4344,.T.);
#5477=ORIENTED_EDGE('',*,*,#4347,.T.);
#5478=ORIENTED_EDGE('',*,*,#4350,.T.);
#5479=ORIENTED_EDGE('',*,*,#4353,.T.);
#5480=ORIENTED_EDGE('',*,*,#4356,.T.);
#5481=ORIENTED_EDGE('',*,*,#4399,.T.);
#5482=ORIENTED_EDGE('',*,*,#4395,.T.);
#5483=ORIENTED_EDGE('',*,*,#4303,.T.);
#5484=ORIENTED_EDGE('',*,*,#4307,.T.);
#5485=ORIENTED_EDGE('',*,*,#4310,.T.);
#5486=ORIENTED_EDGE('',*,*,#4313,.T.);
#5487=ORIENTED_EDGE('',*,*,#4316,.T.);
#5488=ORIENTED_EDGE('',*,*,#4319,.T.);
#5489=ORIENTED_EDGE('',*,*,#4322,.T.);
#5490=ORIENTED_EDGE('',*,*,#4325,.T.);
#5491=ORIENTED_EDGE('',*,*,#4328,.T.);
#5492=ORIENTED_EDGE('',*,*,#4394,.T.);
#5493=ORIENTED_EDGE('',*,*,#4390,.T.);
#5494=ORIENTED_EDGE('',*,*,#4386,.T.);
#5495=ORIENTED_EDGE('',*,*,#4273,.T.);
#5496=ORIENTED_EDGE('',*,*,#4392,.F.);
#5497=ORIENTED_EDGE('',*,*,#4393,.F.);
#5498=ORIENTED_EDGE('',*,*,#4326,.T.);
#5499=ORIENTED_EDGE('',*,*,#4323,.T.);
#5500=ORIENTED_EDGE('',*,*,#4320,.T.);
#5501=ORIENTED_EDGE('',*,*,#4317,.T.);
#5502=ORIENTED_EDGE('',*,*,#4314,.T.);
#5503=ORIENTED_EDGE('',*,*,#4311,.T.);
#5504=ORIENTED_EDGE('',*,*,#4308,.T.);
#5505=ORIENTED_EDGE('',*,*,#4305,.T.);
#5506=ORIENTED_EDGE('',*,*,#4301,.T.);
#5507=ORIENTED_EDGE('',*,*,#4397,.F.);
#5508=ORIENTED_EDGE('',*,*,#4398,.F.);
#5509=ORIENTED_EDGE('',*,*,#4354,.T.);
#5510=ORIENTED_EDGE('',*,*,#4351,.T.);
#5511=ORIENTED_EDGE('',*,*,#4348,.T.);
#5512=ORIENTED_EDGE('',*,*,#4345,.T.);
#5513=ORIENTED_EDGE('',*,*,#4342,.T.);
#5514=ORIENTED_EDGE('',*,*,#4339,.T.);
#5515=ORIENTED_EDGE('',*,*,#4336,.T.);
#5516=ORIENTED_EDGE('',*,*,#4333,.T.);
#5517=ORIENTED_EDGE('',*,*,#4329,.T.);
#5518=ORIENTED_EDGE('',*,*,#4402,.F.);
#5519=ORIENTED_EDGE('',*,*,#4403,.F.);
#5520=ORIENTED_EDGE('',*,*,#4382,.T.);
#5521=ORIENTED_EDGE('',*,*,#4379,.T.);
#5522=ORIENTED_EDGE('',*,*,#4376,.T.);
#5523=ORIENTED_EDGE('',*,*,#4373,.T.);
#5524=ORIENTED_EDGE('',*,*,#4370,.T.);
#5525=ORIENTED_EDGE('',*,*,#4367,.T.);
#5526=ORIENTED_EDGE('',*,*,#4364,.T.);
#5527=ORIENTED_EDGE('',*,*,#4361,.T.);
#5528=ORIENTED_EDGE('',*,*,#4357,.T.);
#5529=ORIENTED_EDGE('',*,*,#4406,.F.);
#5530=ORIENTED_EDGE('',*,*,#4387,.F.);
#5531=ORIENTED_EDGE('',*,*,#4298,.T.);
#5532=ORIENTED_EDGE('',*,*,#4295,.T.);
#5533=ORIENTED_EDGE('',*,*,#4292,.T.);
#5534=ORIENTED_EDGE('',*,*,#4289,.T.);
#5535=ORIENTED_EDGE('',*,*,#4286,.T.);
#5536=ORIENTED_EDGE('',*,*,#4283,.T.);
#5537=ORIENTED_EDGE('',*,*,#4280,.T.);
#5538=ORIENTED_EDGE('',*,*,#4277,.T.);
#5539=ORIENTED_EDGE('',*,*,#4271,.T.);
#5540=ORIENTED_EDGE('',*,*,#4407,.F.);
#5541=ORIENTED_EDGE('',*,*,#4408,.T.);
#5542=ORIENTED_EDGE('',*,*,#4409,.F.);
#5543=ORIENTED_EDGE('',*,*,#4410,.T.);
#5544=ORIENTED_EDGE('',*,*,#4411,.F.);
#5545=ORIENTED_EDGE('',*,*,#4410,.F.);
#5546=ORIENTED_EDGE('',*,*,#4412,.F.);
#5547=ORIENTED_EDGE('',*,*,#4413,.F.);
#5548=ORIENTED_EDGE('',*,*,#4408,.F.);
#5549=ORIENTED_EDGE('',*,*,#4414,.F.);
#5550=ORIENTED_EDGE('',*,*,#4415,.F.);
#5551=ORIENTED_EDGE('',*,*,#4416,.F.);
#5552=ORIENTED_EDGE('',*,*,#4417,.T.);
#5553=ORIENTED_EDGE('',*,*,#4409,.T.);
#5554=ORIENTED_EDGE('',*,*,#4413,.T.);
#5555=ORIENTED_EDGE('',*,*,#4412,.T.);
#5556=ORIENTED_EDGE('',*,*,#4417,.F.);
#5557=ORIENTED_EDGE('',*,*,#4418,.F.);
#5558=ORIENTED_EDGE('',*,*,#4419,.T.);
#5559=ORIENTED_EDGE('',*,*,#4420,.F.);
#5560=ORIENTED_EDGE('',*,*,#4421,.F.);
#5561=ORIENTED_EDGE('',*,*,#4422,.F.);
#5562=ORIENTED_EDGE('',*,*,#4423,.T.);
#5563=ORIENTED_EDGE('',*,*,#4424,.F.);
#5564=ORIENTED_EDGE('',*,*,#4419,.F.);
#5565=ORIENTED_EDGE('',*,*,#4425,.F.);
#5566=ORIENTED_EDGE('',*,*,#4426,.T.);
#5567=ORIENTED_EDGE('',*,*,#4427,.F.);
#5568=ORIENTED_EDGE('',*,*,#4423,.F.);
#5569=ORIENTED_EDGE('',*,*,#4428,.F.);
#5570=ORIENTED_EDGE('',*,*,#4429,.T.);
#5571=ORIENTED_EDGE('',*,*,#4430,.F.);
#5572=ORIENTED_EDGE('',*,*,#4426,.F.);
#5573=ORIENTED_EDGE('',*,*,#4431,.F.);
#5574=ORIENTED_EDGE('',*,*,#4432,.T.);
#5575=ORIENTED_EDGE('',*,*,#4433,.F.);
#5576=ORIENTED_EDGE('',*,*,#4429,.F.);
#5577=ORIENTED_EDGE('',*,*,#4434,.F.);
#5578=ORIENTED_EDGE('',*,*,#4435,.T.);
#5579=ORIENTED_EDGE('',*,*,#4436,.F.);
#5580=ORIENTED_EDGE('',*,*,#4432,.F.);
#5581=ORIENTED_EDGE('',*,*,#4437,.F.);
#5582=ORIENTED_EDGE('',*,*,#4438,.T.);
#5583=ORIENTED_EDGE('',*,*,#4439,.F.);
#5584=ORIENTED_EDGE('',*,*,#4435,.F.);
#5585=ORIENTED_EDGE('',*,*,#4440,.F.);
#5586=ORIENTED_EDGE('',*,*,#4441,.T.);
#5587=ORIENTED_EDGE('',*,*,#4442,.F.);
#5588=ORIENTED_EDGE('',*,*,#4438,.F.);
#5589=ORIENTED_EDGE('',*,*,#4443,.F.);
#5590=ORIENTED_EDGE('',*,*,#4444,.F.);
#5591=ORIENTED_EDGE('',*,*,#4445,.F.);
#5592=ORIENTED_EDGE('',*,*,#4441,.F.);
#5593=ORIENTED_EDGE('',*,*,#4446,.F.);
#5594=ORIENTED_EDGE('',*,*,#4447,.T.);
#5595=ORIENTED_EDGE('',*,*,#4448,.F.);
#5596=ORIENTED_EDGE('',*,*,#4449,.F.);
#5597=ORIENTED_EDGE('',*,*,#4450,.F.);
#5598=ORIENTED_EDGE('',*,*,#4451,.T.);
#5599=ORIENTED_EDGE('',*,*,#4452,.F.);
#5600=ORIENTED_EDGE('',*,*,#4447,.F.);
#5601=ORIENTED_EDGE('',*,*,#4453,.F.);
#5602=ORIENTED_EDGE('',*,*,#4454,.T.);
#5603=ORIENTED_EDGE('',*,*,#4455,.F.);
#5604=ORIENTED_EDGE('',*,*,#4451,.F.);
#5605=ORIENTED_EDGE('',*,*,#4456,.F.);
#5606=ORIENTED_EDGE('',*,*,#4457,.T.);
#5607=ORIENTED_EDGE('',*,*,#4458,.F.);
#5608=ORIENTED_EDGE('',*,*,#4454,.F.);
#5609=ORIENTED_EDGE('',*,*,#4459,.F.);
#5610=ORIENTED_EDGE('',*,*,#4460,.T.);
#5611=ORIENTED_EDGE('',*,*,#4461,.F.);
#5612=ORIENTED_EDGE('',*,*,#4457,.F.);
#5613=ORIENTED_EDGE('',*,*,#4407,.T.);
#5614=ORIENTED_EDGE('',*,*,#4462,.F.);
#5615=ORIENTED_EDGE('',*,*,#4463,.T.);
#5616=ORIENTED_EDGE('',*,*,#4464,.F.);
#5617=ORIENTED_EDGE('',*,*,#4460,.F.);
#5618=ORIENTED_EDGE('',*,*,#4465,.F.);
#5619=ORIENTED_EDGE('',*,*,#4466,.T.);
#5620=ORIENTED_EDGE('',*,*,#4467,.F.);
#5621=ORIENTED_EDGE('',*,*,#4463,.F.);
#5622=ORIENTED_EDGE('',*,*,#4468,.F.);
#5623=ORIENTED_EDGE('',*,*,#4469,.T.);
#5624=ORIENTED_EDGE('',*,*,#4470,.F.);
#5625=ORIENTED_EDGE('',*,*,#4466,.F.);
#5626=ORIENTED_EDGE('',*,*,#4471,.F.);
#5627=ORIENTED_EDGE('',*,*,#4472,.F.);
#5628=ORIENTED_EDGE('',*,*,#4473,.F.);
#5629=ORIENTED_EDGE('',*,*,#4469,.F.);
#5630=ORIENTED_EDGE('',*,*,#4474,.F.);
#5631=ORIENTED_EDGE('',*,*,#4475,.T.);
#5632=ORIENTED_EDGE('',*,*,#4476,.F.);
#5633=ORIENTED_EDGE('',*,*,#4477,.F.);
#5634=ORIENTED_EDGE('',*,*,#4478,.F.);
#5635=ORIENTED_EDGE('',*,*,#4479,.T.);
#5636=ORIENTED_EDGE('',*,*,#4480,.F.);
#5637=ORIENTED_EDGE('',*,*,#4475,.F.);
#5638=ORIENTED_EDGE('',*,*,#4481,.F.);
#5639=ORIENTED_EDGE('',*,*,#4482,.T.);
#5640=ORIENTED_EDGE('',*,*,#4483,.F.);
#5641=ORIENTED_EDGE('',*,*,#4479,.F.);
#5642=ORIENTED_EDGE('',*,*,#4484,.F.);
#5643=ORIENTED_EDGE('',*,*,#4485,.T.);
#5644=ORIENTED_EDGE('',*,*,#4486,.F.);
#5645=ORIENTED_EDGE('',*,*,#4482,.F.);
#5646=ORIENTED_EDGE('',*,*,#4487,.F.);
#5647=ORIENTED_EDGE('',*,*,#4488,.T.);
#5648=ORIENTED_EDGE('',*,*,#4489,.F.);
#5649=ORIENTED_EDGE('',*,*,#4485,.F.);
#5650=ORIENTED_EDGE('',*,*,#4490,.F.);
#5651=ORIENTED_EDGE('',*,*,#4491,.T.);
#5652=ORIENTED_EDGE('',*,*,#4492,.F.);
#5653=ORIENTED_EDGE('',*,*,#4488,.F.);
#5654=ORIENTED_EDGE('',*,*,#4493,.F.);
#5655=ORIENTED_EDGE('',*,*,#4494,.T.);
#5656=ORIENTED_EDGE('',*,*,#4495,.F.);
#5657=ORIENTED_EDGE('',*,*,#4491,.F.);
#5658=ORIENTED_EDGE('',*,*,#4496,.F.);
#5659=ORIENTED_EDGE('',*,*,#4497,.T.);
#5660=ORIENTED_EDGE('',*,*,#4498,.F.);
#5661=ORIENTED_EDGE('',*,*,#4494,.F.);
#5662=ORIENTED_EDGE('',*,*,#4499,.F.);
#5663=ORIENTED_EDGE('',*,*,#4500,.F.);
#5664=ORIENTED_EDGE('',*,*,#4501,.F.);
#5665=ORIENTED_EDGE('',*,*,#4497,.F.);
#5666=ORIENTED_EDGE('',*,*,#4502,.F.);
#5667=ORIENTED_EDGE('',*,*,#4503,.T.);
#5668=ORIENTED_EDGE('',*,*,#4504,.F.);
#5669=ORIENTED_EDGE('',*,*,#4505,.F.);
#5670=ORIENTED_EDGE('',*,*,#4506,.F.);
#5671=ORIENTED_EDGE('',*,*,#4507,.T.);
#5672=ORIENTED_EDGE('',*,*,#4508,.F.);
#5673=ORIENTED_EDGE('',*,*,#4503,.F.);
#5674=ORIENTED_EDGE('',*,*,#4509,.F.);
#5675=ORIENTED_EDGE('',*,*,#4510,.T.);
#5676=ORIENTED_EDGE('',*,*,#4511,.F.);
#5677=ORIENTED_EDGE('',*,*,#4507,.F.);
#5678=ORIENTED_EDGE('',*,*,#4512,.F.);
#5679=ORIENTED_EDGE('',*,*,#4513,.T.);
#5680=ORIENTED_EDGE('',*,*,#4514,.F.);
#5681=ORIENTED_EDGE('',*,*,#4510,.F.);
#5682=ORIENTED_EDGE('',*,*,#4515,.F.);
#5683=ORIENTED_EDGE('',*,*,#4516,.T.);
#5684=ORIENTED_EDGE('',*,*,#4517,.F.);
#5685=ORIENTED_EDGE('',*,*,#4513,.F.);
#5686=ORIENTED_EDGE('',*,*,#4411,.T.);
#5687=ORIENTED_EDGE('',*,*,#4518,.F.);
#5688=ORIENTED_EDGE('',*,*,#4519,.T.);
#5689=ORIENTED_EDGE('',*,*,#4520,.F.);
#5690=ORIENTED_EDGE('',*,*,#4516,.F.);
#5691=ORIENTED_EDGE('',*,*,#4521,.F.);
#5692=ORIENTED_EDGE('',*,*,#4522,.T.);
#5693=ORIENTED_EDGE('',*,*,#4523,.F.);
#5694=ORIENTED_EDGE('',*,*,#4519,.F.);
#5695=ORIENTED_EDGE('',*,*,#4524,.F.);
#5696=ORIENTED_EDGE('',*,*,#4525,.T.);
#5697=ORIENTED_EDGE('',*,*,#4526,.F.);
#5698=ORIENTED_EDGE('',*,*,#4522,.F.);
#5699=ORIENTED_EDGE('',*,*,#4527,.F.);
#5700=ORIENTED_EDGE('',*,*,#4528,.F.);
#5701=ORIENTED_EDGE('',*,*,#4529,.F.);
#5702=ORIENTED_EDGE('',*,*,#4525,.F.);
#5703=ORIENTED_EDGE('',*,*,#4414,.T.);
#5704=ORIENTED_EDGE('',*,*,#4530,.T.);
#5705=ORIENTED_EDGE('',*,*,#4531,.F.);
#5706=ORIENTED_EDGE('',*,*,#4530,.F.);
#5707=ORIENTED_EDGE('',*,*,#4415,.T.);
#5708=ORIENTED_EDGE('',*,*,#4444,.T.);
#5709=ORIENTED_EDGE('',*,*,#4532,.T.);
#5710=ORIENTED_EDGE('',*,*,#4533,.T.);
#5711=ORIENTED_EDGE('',*,*,#4534,.F.);
#5712=ORIENTED_EDGE('',*,*,#4421,.T.);
#5713=ORIENTED_EDGE('',*,*,#4535,.F.);
#5714=ORIENTED_EDGE('',*,*,#4536,.F.);
#5715=ORIENTED_EDGE('',*,*,#4537,.T.);
#5716=ORIENTED_EDGE('',*,*,#4472,.T.);
#5717=ORIENTED_EDGE('',*,*,#4538,.T.);
#5718=ORIENTED_EDGE('',*,*,#4536,.T.);
#5719=ORIENTED_EDGE('',*,*,#4539,.F.);
#5720=ORIENTED_EDGE('',*,*,#4449,.T.);
#5721=ORIENTED_EDGE('',*,*,#4540,.F.);
#5722=ORIENTED_EDGE('',*,*,#4541,.F.);
#5723=ORIENTED_EDGE('',*,*,#4542,.T.);
#5724=ORIENTED_EDGE('',*,*,#4500,.T.);
#5725=ORIENTED_EDGE('',*,*,#4543,.T.);
#5726=ORIENTED_EDGE('',*,*,#4541,.T.);
#5727=ORIENTED_EDGE('',*,*,#4544,.F.);
#5728=ORIENTED_EDGE('',*,*,#4477,.T.);
#5729=ORIENTED_EDGE('',*,*,#4545,.F.);
#5730=ORIENTED_EDGE('',*,*,#4546,.F.);
#5731=ORIENTED_EDGE('',*,*,#4547,.T.);
#5732=ORIENTED_EDGE('',*,*,#4528,.T.);
#5733=ORIENTED_EDGE('',*,*,#4548,.T.);
#5734=ORIENTED_EDGE('',*,*,#4546,.T.);
#5735=ORIENTED_EDGE('',*,*,#4549,.F.);
#5736=ORIENTED_EDGE('',*,*,#4505,.T.);
#5737=ORIENTED_EDGE('',*,*,#4550,.F.);
#5738=ORIENTED_EDGE('',*,*,#4533,.F.);
#5739=ORIENTED_EDGE('',*,*,#4551,.T.);
#5740=ORIENTED_EDGE('',*,*,#4420,.T.);
#5741=ORIENTED_EDGE('',*,*,#4424,.T.);
#5742=ORIENTED_EDGE('',*,*,#4427,.T.);
#5743=ORIENTED_EDGE('',*,*,#4430,.T.);
#5744=ORIENTED_EDGE('',*,*,#4433,.T.);
#5745=ORIENTED_EDGE('',*,*,#4436,.T.);
#5746=ORIENTED_EDGE('',*,*,#4439,.T.);
#5747=ORIENTED_EDGE('',*,*,#4442,.T.);
#5748=ORIENTED_EDGE('',*,*,#4445,.T.);
#5749=ORIENTED_EDGE('',*,*,#4534,.T.);
#5750=ORIENTED_EDGE('',*,*,#4550,.T.);
#5751=ORIENTED_EDGE('',*,*,#4504,.T.);
#5752=ORIENTED_EDGE('',*,*,#4508,.T.);
#5753=ORIENTED_EDGE('',*,*,#4511,.T.);
#5754=ORIENTED_EDGE('',*,*,#4514,.T.);
#5755=ORIENTED_EDGE('',*,*,#4517,.T.);
#5756=ORIENTED_EDGE('',*,*,#4520,.T.);
#5757=ORIENTED_EDGE('',*,*,#4523,.T.);
#5758=ORIENTED_EDGE('',*,*,#4526,.T.);
#5759=ORIENTED_EDGE('',*,*,#4529,.T.);
#5760=ORIENTED_EDGE('',*,*,#4549,.T.);
#5761=ORIENTED_EDGE('',*,*,#4545,.T.);
#5762=ORIENTED_EDGE('',*,*,#4476,.T.);
#5763=ORIENTED_EDGE('',*,*,#4480,.T.);
#5764=ORIENTED_EDGE('',*,*,#4483,.T.);
#5765=ORIENTED_EDGE('',*,*,#4486,.T.);
#5766=ORIENTED_EDGE('',*,*,#4489,.T.);
#5767=ORIENTED_EDGE('',*,*,#4492,.T.);
#5768=ORIENTED_EDGE('',*,*,#4495,.T.);
#5769=ORIENTED_EDGE('',*,*,#4498,.T.);
#5770=ORIENTED_EDGE('',*,*,#4501,.T.);
#5771=ORIENTED_EDGE('',*,*,#4544,.T.);
#5772=ORIENTED_EDGE('',*,*,#4540,.T.);
#5773=ORIENTED_EDGE('',*,*,#4448,.T.);
#5774=ORIENTED_EDGE('',*,*,#4452,.T.);
#5775=ORIENTED_EDGE('',*,*,#4455,.T.);
#5776=ORIENTED_EDGE('',*,*,#4458,.T.);
#5777=ORIENTED_EDGE('',*,*,#4461,.T.);
#5778=ORIENTED_EDGE('',*,*,#4464,.T.);
#5779=ORIENTED_EDGE('',*,*,#4467,.T.);
#5780=ORIENTED_EDGE('',*,*,#4470,.T.);
#5781=ORIENTED_EDGE('',*,*,#4473,.T.);
#5782=ORIENTED_EDGE('',*,*,#4539,.T.);
#5783=ORIENTED_EDGE('',*,*,#4535,.T.);
#5784=ORIENTED_EDGE('',*,*,#4531,.T.);
#5785=ORIENTED_EDGE('',*,*,#4418,.T.);
#5786=ORIENTED_EDGE('',*,*,#4537,.F.);
#5787=ORIENTED_EDGE('',*,*,#4538,.F.);
#5788=ORIENTED_EDGE('',*,*,#4471,.T.);
#5789=ORIENTED_EDGE('',*,*,#4468,.T.);
#5790=ORIENTED_EDGE('',*,*,#4465,.T.);
#5791=ORIENTED_EDGE('',*,*,#4462,.T.);
#5792=ORIENTED_EDGE('',*,*,#4459,.T.);
#5793=ORIENTED_EDGE('',*,*,#4456,.T.);
#5794=ORIENTED_EDGE('',*,*,#4453,.T.);
#5795=ORIENTED_EDGE('',*,*,#4450,.T.);
#5796=ORIENTED_EDGE('',*,*,#4446,.T.);
#5797=ORIENTED_EDGE('',*,*,#4542,.F.);
#5798=ORIENTED_EDGE('',*,*,#4543,.F.);
#5799=ORIENTED_EDGE('',*,*,#4499,.T.);
#5800=ORIENTED_EDGE('',*,*,#4496,.T.);
#5801=ORIENTED_EDGE('',*,*,#4493,.T.);
#5802=ORIENTED_EDGE('',*,*,#4490,.T.);
#5803=ORIENTED_EDGE('',*,*,#4487,.T.);
#5804=ORIENTED_EDGE('',*,*,#4484,.T.);
#5805=ORIENTED_EDGE('',*,*,#4481,.T.);
#5806=ORIENTED_EDGE('',*,*,#4478,.T.);
#5807=ORIENTED_EDGE('',*,*,#4474,.T.);
#5808=ORIENTED_EDGE('',*,*,#4547,.F.);
#5809=ORIENTED_EDGE('',*,*,#4548,.F.);
#5810=ORIENTED_EDGE('',*,*,#4527,.T.);
#5811=ORIENTED_EDGE('',*,*,#4524,.T.);
#5812=ORIENTED_EDGE('',*,*,#4521,.T.);
#5813=ORIENTED_EDGE('',*,*,#4518,.T.);
#5814=ORIENTED_EDGE('',*,*,#4515,.T.);
#5815=ORIENTED_EDGE('',*,*,#4512,.T.);
#5816=ORIENTED_EDGE('',*,*,#4509,.T.);
#5817=ORIENTED_EDGE('',*,*,#4506,.T.);
#5818=ORIENTED_EDGE('',*,*,#4502,.T.);
#5819=ORIENTED_EDGE('',*,*,#4551,.F.);
#5820=ORIENTED_EDGE('',*,*,#4532,.F.);
#5821=ORIENTED_EDGE('',*,*,#4443,.T.);
#5822=ORIENTED_EDGE('',*,*,#4440,.T.);
#5823=ORIENTED_EDGE('',*,*,#4437,.T.);
#5824=ORIENTED_EDGE('',*,*,#4434,.T.);
#5825=ORIENTED_EDGE('',*,*,#4431,.T.);
#5826=ORIENTED_EDGE('',*,*,#4428,.T.);
#5827=ORIENTED_EDGE('',*,*,#4425,.T.);
#5828=ORIENTED_EDGE('',*,*,#4422,.T.);
#5829=ORIENTED_EDGE('',*,*,#4416,.T.);
#5830=ORIENTED_EDGE('',*,*,#4552,.F.);
#5831=ORIENTED_EDGE('',*,*,#4553,.T.);
#5832=ORIENTED_EDGE('',*,*,#4554,.F.);
#5833=ORIENTED_EDGE('',*,*,#4555,.F.);
#5834=ORIENTED_EDGE('',*,*,#4556,.F.);
#5835=ORIENTED_EDGE('',*,*,#4557,.T.);
#5836=ORIENTED_EDGE('',*,*,#4558,.F.);
#5837=ORIENTED_EDGE('',*,*,#4553,.F.);
#5838=ORIENTED_EDGE('',*,*,#4559,.F.);
#5839=ORIENTED_EDGE('',*,*,#4560,.T.);
#5840=ORIENTED_EDGE('',*,*,#4561,.F.);
#5841=ORIENTED_EDGE('',*,*,#4557,.F.);
#5842=ORIENTED_EDGE('',*,*,#4562,.F.);
#5843=ORIENTED_EDGE('',*,*,#4563,.T.);
#5844=ORIENTED_EDGE('',*,*,#4564,.F.);
#5845=ORIENTED_EDGE('',*,*,#4560,.F.);
#5846=ORIENTED_EDGE('',*,*,#4565,.F.);
#5847=ORIENTED_EDGE('',*,*,#4566,.T.);
#5848=ORIENTED_EDGE('',*,*,#4567,.F.);
#5849=ORIENTED_EDGE('',*,*,#4563,.F.);
#5850=ORIENTED_EDGE('',*,*,#4568,.F.);
#5851=ORIENTED_EDGE('',*,*,#4569,.T.);
#5852=ORIENTED_EDGE('',*,*,#4570,.F.);
#5853=ORIENTED_EDGE('',*,*,#4566,.F.);
#5854=ORIENTED_EDGE('',*,*,#4571,.F.);
#5855=ORIENTED_EDGE('',*,*,#4572,.T.);
#5856=ORIENTED_EDGE('',*,*,#4573,.F.);
#5857=ORIENTED_EDGE('',*,*,#4569,.F.);
#5858=ORIENTED_EDGE('',*,*,#4574,.F.);
#5859=ORIENTED_EDGE('',*,*,#4575,.T.);
#5860=ORIENTED_EDGE('',*,*,#4576,.F.);
#5861=ORIENTED_EDGE('',*,*,#4572,.F.);
#5862=ORIENTED_EDGE('',*,*,#4577,.F.);
#5863=ORIENTED_EDGE('',*,*,#4578,.F.);
#5864=ORIENTED_EDGE('',*,*,#4579,.F.);
#5865=ORIENTED_EDGE('',*,*,#4575,.F.);
#5866=ORIENTED_EDGE('',*,*,#4580,.F.);
#5867=ORIENTED_EDGE('',*,*,#4581,.T.);
#5868=ORIENTED_EDGE('',*,*,#4582,.F.);
#5869=ORIENTED_EDGE('',*,*,#4583,.F.);
#5870=ORIENTED_EDGE('',*,*,#4584,.F.);
#5871=ORIENTED_EDGE('',*,*,#4585,.T.);
#5872=ORIENTED_EDGE('',*,*,#4586,.F.);
#5873=ORIENTED_EDGE('',*,*,#4581,.F.);
#5874=ORIENTED_EDGE('',*,*,#4587,.F.);
#5875=ORIENTED_EDGE('',*,*,#4588,.T.);
#5876=ORIENTED_EDGE('',*,*,#4589,.F.);
#5877=ORIENTED_EDGE('',*,*,#4585,.F.);
#5878=ORIENTED_EDGE('',*,*,#4590,.F.);
#5879=ORIENTED_EDGE('',*,*,#4591,.T.);
#5880=ORIENTED_EDGE('',*,*,#4592,.F.);
#5881=ORIENTED_EDGE('',*,*,#4588,.F.);
#5882=ORIENTED_EDGE('',*,*,#4593,.F.);
#5883=ORIENTED_EDGE('',*,*,#4594,.T.);
#5884=ORIENTED_EDGE('',*,*,#4595,.F.);
#5885=ORIENTED_EDGE('',*,*,#4591,.F.);
#5886=ORIENTED_EDGE('',*,*,#4596,.F.);
#5887=ORIENTED_EDGE('',*,*,#4597,.T.);
#5888=ORIENTED_EDGE('',*,*,#4598,.F.);
#5889=ORIENTED_EDGE('',*,*,#4594,.F.);
#5890=ORIENTED_EDGE('',*,*,#4599,.F.);
#5891=ORIENTED_EDGE('',*,*,#4600,.T.);
#5892=ORIENTED_EDGE('',*,*,#4601,.F.);
#5893=ORIENTED_EDGE('',*,*,#4597,.F.);
#5894=ORIENTED_EDGE('',*,*,#4602,.F.);
#5895=ORIENTED_EDGE('',*,*,#4603,.T.);
#5896=ORIENTED_EDGE('',*,*,#4604,.F.);
#5897=ORIENTED_EDGE('',*,*,#4600,.F.);
#5898=ORIENTED_EDGE('',*,*,#4605,.F.);
#5899=ORIENTED_EDGE('',*,*,#4606,.F.);
#5900=ORIENTED_EDGE('',*,*,#4607,.F.);
#5901=ORIENTED_EDGE('',*,*,#4603,.F.);
#5902=ORIENTED_EDGE('',*,*,#4608,.F.);
#5903=ORIENTED_EDGE('',*,*,#4609,.T.);
#5904=ORIENTED_EDGE('',*,*,#4610,.F.);
#5905=ORIENTED_EDGE('',*,*,#4611,.F.);
#5906=ORIENTED_EDGE('',*,*,#4612,.F.);
#5907=ORIENTED_EDGE('',*,*,#4613,.T.);
#5908=ORIENTED_EDGE('',*,*,#4614,.F.);
#5909=ORIENTED_EDGE('',*,*,#4609,.F.);
#5910=ORIENTED_EDGE('',*,*,#4615,.F.);
#5911=ORIENTED_EDGE('',*,*,#4616,.T.);
#5912=ORIENTED_EDGE('',*,*,#4617,.F.);
#5913=ORIENTED_EDGE('',*,*,#4613,.F.);
#5914=ORIENTED_EDGE('',*,*,#4618,.F.);
#5915=ORIENTED_EDGE('',*,*,#4619,.T.);
#5916=ORIENTED_EDGE('',*,*,#4620,.F.);
#5917=ORIENTED_EDGE('',*,*,#4616,.F.);
#5918=ORIENTED_EDGE('',*,*,#4621,.F.);
#5919=ORIENTED_EDGE('',*,*,#4622,.T.);
#5920=ORIENTED_EDGE('',*,*,#4623,.F.);
#5921=ORIENTED_EDGE('',*,*,#4619,.F.);
#5922=ORIENTED_EDGE('',*,*,#4624,.F.);
#5923=ORIENTED_EDGE('',*,*,#4625,.T.);
#5924=ORIENTED_EDGE('',*,*,#4626,.F.);
#5925=ORIENTED_EDGE('',*,*,#4622,.F.);
#5926=ORIENTED_EDGE('',*,*,#4627,.F.);
#5927=ORIENTED_EDGE('',*,*,#4628,.T.);
#5928=ORIENTED_EDGE('',*,*,#4629,.F.);
#5929=ORIENTED_EDGE('',*,*,#4625,.F.);
#5930=ORIENTED_EDGE('',*,*,#4630,.F.);
#5931=ORIENTED_EDGE('',*,*,#4631,.T.);
#5932=ORIENTED_EDGE('',*,*,#4632,.F.);
#5933=ORIENTED_EDGE('',*,*,#4628,.F.);
#5934=ORIENTED_EDGE('',*,*,#4633,.F.);
#5935=ORIENTED_EDGE('',*,*,#4634,.F.);
#5936=ORIENTED_EDGE('',*,*,#4635,.F.);
#5937=ORIENTED_EDGE('',*,*,#4631,.F.);
#5938=ORIENTED_EDGE('',*,*,#4636,.F.);
#5939=ORIENTED_EDGE('',*,*,#4637,.T.);
#5940=ORIENTED_EDGE('',*,*,#4638,.F.);
#5941=ORIENTED_EDGE('',*,*,#4639,.F.);
#5942=ORIENTED_EDGE('',*,*,#4640,.F.);
#5943=ORIENTED_EDGE('',*,*,#4641,.T.);
#5944=ORIENTED_EDGE('',*,*,#4642,.F.);
#5945=ORIENTED_EDGE('',*,*,#4637,.F.);
#5946=ORIENTED_EDGE('',*,*,#4643,.F.);
#5947=ORIENTED_EDGE('',*,*,#4644,.T.);
#5948=ORIENTED_EDGE('',*,*,#4645,.F.);
#5949=ORIENTED_EDGE('',*,*,#4641,.F.);
#5950=ORIENTED_EDGE('',*,*,#4646,.F.);
#5951=ORIENTED_EDGE('',*,*,#4647,.T.);
#5952=ORIENTED_EDGE('',*,*,#4648,.F.);
#5953=ORIENTED_EDGE('',*,*,#4644,.F.);
#5954=ORIENTED_EDGE('',*,*,#4649,.F.);
#5955=ORIENTED_EDGE('',*,*,#4650,.T.);
#5956=ORIENTED_EDGE('',*,*,#4651,.F.);
#5957=ORIENTED_EDGE('',*,*,#4647,.F.);
#5958=ORIENTED_EDGE('',*,*,#4652,.F.);
#5959=ORIENTED_EDGE('',*,*,#4653,.T.);
#5960=ORIENTED_EDGE('',*,*,#4654,.F.);
#5961=ORIENTED_EDGE('',*,*,#4650,.F.);
#5962=ORIENTED_EDGE('',*,*,#4655,.F.);
#5963=ORIENTED_EDGE('',*,*,#4656,.T.);
#5964=ORIENTED_EDGE('',*,*,#4657,.F.);
#5965=ORIENTED_EDGE('',*,*,#4653,.F.);
#5966=ORIENTED_EDGE('',*,*,#4658,.F.);
#5967=ORIENTED_EDGE('',*,*,#4659,.T.);
#5968=ORIENTED_EDGE('',*,*,#4660,.F.);
#5969=ORIENTED_EDGE('',*,*,#4656,.F.);
#5970=ORIENTED_EDGE('',*,*,#4661,.F.);
#5971=ORIENTED_EDGE('',*,*,#4662,.F.);
#5972=ORIENTED_EDGE('',*,*,#4663,.F.);
#5973=ORIENTED_EDGE('',*,*,#4659,.F.);
#5974=ORIENTED_EDGE('',*,*,#4664,.F.);
#5975=ORIENTED_EDGE('',*,*,#4665,.T.);
#5976=ORIENTED_EDGE('',*,*,#4666,.F.);
#5977=ORIENTED_EDGE('',*,*,#4665,.F.);
#5978=ORIENTED_EDGE('',*,*,#4578,.T.);
#5979=ORIENTED_EDGE('',*,*,#4667,.T.);
#5980=ORIENTED_EDGE('',*,*,#4668,.T.);
#5981=ORIENTED_EDGE('',*,*,#4669,.F.);
#5982=ORIENTED_EDGE('',*,*,#4555,.T.);
#5983=ORIENTED_EDGE('',*,*,#4670,.F.);
#5984=ORIENTED_EDGE('',*,*,#4671,.F.);
#5985=ORIENTED_EDGE('',*,*,#4672,.T.);
#5986=ORIENTED_EDGE('',*,*,#4606,.T.);
#5987=ORIENTED_EDGE('',*,*,#4673,.T.);
#5988=ORIENTED_EDGE('',*,*,#4671,.T.);
#5989=ORIENTED_EDGE('',*,*,#4674,.F.);
#5990=ORIENTED_EDGE('',*,*,#4583,.T.);
#5991=ORIENTED_EDGE('',*,*,#4675,.F.);
#5992=ORIENTED_EDGE('',*,*,#4676,.F.);
#5993=ORIENTED_EDGE('',*,*,#4677,.T.);
#5994=ORIENTED_EDGE('',*,*,#4634,.T.);
#5995=ORIENTED_EDGE('',*,*,#4678,.T.);
#5996=ORIENTED_EDGE('',*,*,#4676,.T.);
#5997=ORIENTED_EDGE('',*,*,#4679,.F.);
#5998=ORIENTED_EDGE('',*,*,#4611,.T.);
#5999=ORIENTED_EDGE('',*,*,#4680,.F.);
#6000=ORIENTED_EDGE('',*,*,#4681,.F.);
#6001=ORIENTED_EDGE('',*,*,#4682,.T.);
#6002=ORIENTED_EDGE('',*,*,#4662,.T.);
#6003=ORIENTED_EDGE('',*,*,#4683,.T.);
#6004=ORIENTED_EDGE('',*,*,#4681,.T.);
#6005=ORIENTED_EDGE('',*,*,#4684,.F.);
#6006=ORIENTED_EDGE('',*,*,#4639,.T.);
#6007=ORIENTED_EDGE('',*,*,#4685,.F.);
#6008=ORIENTED_EDGE('',*,*,#4668,.F.);
#6009=ORIENTED_EDGE('',*,*,#4686,.T.);
#6010=ORIENTED_EDGE('',*,*,#4554,.T.);
#6011=ORIENTED_EDGE('',*,*,#4558,.T.);
#6012=ORIENTED_EDGE('',*,*,#4561,.T.);
#6013=ORIENTED_EDGE('',*,*,#4564,.T.);
#6014=ORIENTED_EDGE('',*,*,#4567,.T.);
#6015=ORIENTED_EDGE('',*,*,#4570,.T.);
#6016=ORIENTED_EDGE('',*,*,#4573,.T.);
#6017=ORIENTED_EDGE('',*,*,#4576,.T.);
#6018=ORIENTED_EDGE('',*,*,#4579,.T.);
#6019=ORIENTED_EDGE('',*,*,#4669,.T.);
#6020=ORIENTED_EDGE('',*,*,#4685,.T.);
#6021=ORIENTED_EDGE('',*,*,#4638,.T.);
#6022=ORIENTED_EDGE('',*,*,#4642,.T.);
#6023=ORIENTED_EDGE('',*,*,#4645,.T.);
#6024=ORIENTED_EDGE('',*,*,#4648,.T.);
#6025=ORIENTED_EDGE('',*,*,#4651,.T.);
#6026=ORIENTED_EDGE('',*,*,#4654,.T.);
#6027=ORIENTED_EDGE('',*,*,#4657,.T.);
#6028=ORIENTED_EDGE('',*,*,#4660,.T.);
#6029=ORIENTED_EDGE('',*,*,#4663,.T.);
#6030=ORIENTED_EDGE('',*,*,#4684,.T.);
#6031=ORIENTED_EDGE('',*,*,#4680,.T.);
#6032=ORIENTED_EDGE('',*,*,#4610,.T.);
#6033=ORIENTED_EDGE('',*,*,#4614,.T.);
#6034=ORIENTED_EDGE('',*,*,#4617,.T.);
#6035=ORIENTED_EDGE('',*,*,#4620,.T.);
#6036=ORIENTED_EDGE('',*,*,#4623,.T.);
#6037=ORIENTED_EDGE('',*,*,#4626,.T.);
#6038=ORIENTED_EDGE('',*,*,#4629,.T.);
#6039=ORIENTED_EDGE('',*,*,#4632,.T.);
#6040=ORIENTED_EDGE('',*,*,#4635,.T.);
#6041=ORIENTED_EDGE('',*,*,#4679,.T.);
#6042=ORIENTED_EDGE('',*,*,#4675,.T.);
#6043=ORIENTED_EDGE('',*,*,#4582,.T.);
#6044=ORIENTED_EDGE('',*,*,#4586,.T.);
#6045=ORIENTED_EDGE('',*,*,#4589,.T.);
#6046=ORIENTED_EDGE('',*,*,#4592,.T.);
#6047=ORIENTED_EDGE('',*,*,#4595,.T.);
#6048=ORIENTED_EDGE('',*,*,#4598,.T.);
#6049=ORIENTED_EDGE('',*,*,#4601,.T.);
#6050=ORIENTED_EDGE('',*,*,#4604,.T.);
#6051=ORIENTED_EDGE('',*,*,#4607,.T.);
#6052=ORIENTED_EDGE('',*,*,#4674,.T.);
#6053=ORIENTED_EDGE('',*,*,#4670,.T.);
#6054=ORIENTED_EDGE('',*,*,#4666,.T.);
#6055=ORIENTED_EDGE('',*,*,#4552,.T.);
#6056=ORIENTED_EDGE('',*,*,#4672,.F.);
#6057=ORIENTED_EDGE('',*,*,#4673,.F.);
#6058=ORIENTED_EDGE('',*,*,#4605,.T.);
#6059=ORIENTED_EDGE('',*,*,#4602,.T.);
#6060=ORIENTED_EDGE('',*,*,#4599,.T.);
#6061=ORIENTED_EDGE('',*,*,#4596,.T.);
#6062=ORIENTED_EDGE('',*,*,#4593,.T.);
#6063=ORIENTED_EDGE('',*,*,#4590,.T.);
#6064=ORIENTED_EDGE('',*,*,#4587,.T.);
#6065=ORIENTED_EDGE('',*,*,#4584,.T.);
#6066=ORIENTED_EDGE('',*,*,#4580,.T.);
#6067=ORIENTED_EDGE('',*,*,#4677,.F.);
#6068=ORIENTED_EDGE('',*,*,#4678,.F.);
#6069=ORIENTED_EDGE('',*,*,#4633,.T.);
#6070=ORIENTED_EDGE('',*,*,#4630,.T.);
#6071=ORIENTED_EDGE('',*,*,#4627,.T.);
#6072=ORIENTED_EDGE('',*,*,#4624,.T.);
#6073=ORIENTED_EDGE('',*,*,#4621,.T.);
#6074=ORIENTED_EDGE('',*,*,#4618,.T.);
#6075=ORIENTED_EDGE('',*,*,#4615,.T.);
#6076=ORIENTED_EDGE('',*,*,#4612,.T.);
#6077=ORIENTED_EDGE('',*,*,#4608,.T.);
#6078=ORIENTED_EDGE('',*,*,#4682,.F.);
#6079=ORIENTED_EDGE('',*,*,#4683,.F.);
#6080=ORIENTED_EDGE('',*,*,#4661,.T.);
#6081=ORIENTED_EDGE('',*,*,#4658,.T.);
#6082=ORIENTED_EDGE('',*,*,#4655,.T.);
#6083=ORIENTED_EDGE('',*,*,#4652,.T.);
#6084=ORIENTED_EDGE('',*,*,#4649,.T.);
#6085=ORIENTED_EDGE('',*,*,#4646,.T.);
#6086=ORIENTED_EDGE('',*,*,#4643,.T.);
#6087=ORIENTED_EDGE('',*,*,#4640,.T.);
#6088=ORIENTED_EDGE('',*,*,#4636,.T.);
#6089=ORIENTED_EDGE('',*,*,#4686,.F.);
#6090=ORIENTED_EDGE('',*,*,#4667,.F.);
#6091=ORIENTED_EDGE('',*,*,#4577,.T.);
#6092=ORIENTED_EDGE('',*,*,#4574,.T.);
#6093=ORIENTED_EDGE('',*,*,#4571,.T.);
#6094=ORIENTED_EDGE('',*,*,#4568,.T.);
#6095=ORIENTED_EDGE('',*,*,#4565,.T.);
#6096=ORIENTED_EDGE('',*,*,#4562,.T.);
#6097=ORIENTED_EDGE('',*,*,#4559,.T.);
#6098=ORIENTED_EDGE('',*,*,#4556,.T.);
#6099=ORIENTED_EDGE('',*,*,#4664,.T.);
#6100=ORIENTED_EDGE('',*,*,#4687,.T.);
#6101=ORIENTED_EDGE('',*,*,#4688,.T.);
#6102=ORIENTED_EDGE('',*,*,#4689,.T.);
#6103=ORIENTED_EDGE('',*,*,#4690,.F.);
#6104=ORIENTED_EDGE('',*,*,#4691,.T.);
#6105=ORIENTED_EDGE('',*,*,#4692,.T.);
#6106=ORIENTED_EDGE('',*,*,#4693,.T.);
#6107=ORIENTED_EDGE('',*,*,#4688,.F.);
#6108=ORIENTED_EDGE('',*,*,#4694,.T.);
#6109=ORIENTED_EDGE('',*,*,#4695,.T.);
#6110=ORIENTED_EDGE('',*,*,#4696,.T.);
#6111=ORIENTED_EDGE('',*,*,#4692,.F.);
#6112=ORIENTED_EDGE('',*,*,#4697,.T.);
#6113=ORIENTED_EDGE('',*,*,#4698,.T.);
#6114=ORIENTED_EDGE('',*,*,#4699,.T.);
#6115=ORIENTED_EDGE('',*,*,#4695,.F.);
#6116=ORIENTED_EDGE('',*,*,#4700,.T.);
#6117=ORIENTED_EDGE('',*,*,#4701,.T.);
#6118=ORIENTED_EDGE('',*,*,#4702,.T.);
#6119=ORIENTED_EDGE('',*,*,#4698,.F.);
#6120=ORIENTED_EDGE('',*,*,#4703,.T.);
#6121=ORIENTED_EDGE('',*,*,#4690,.T.);
#6122=ORIENTED_EDGE('',*,*,#4704,.T.);
#6123=ORIENTED_EDGE('',*,*,#4701,.F.);
#6124=ORIENTED_EDGE('',*,*,#4703,.F.);
#6125=ORIENTED_EDGE('',*,*,#4700,.F.);
#6126=ORIENTED_EDGE('',*,*,#4697,.F.);
#6127=ORIENTED_EDGE('',*,*,#4694,.F.);
#6128=ORIENTED_EDGE('',*,*,#4691,.F.);
#6129=ORIENTED_EDGE('',*,*,#4687,.F.);
#6130=ORIENTED_EDGE('',*,*,#4704,.F.);
#6131=ORIENTED_EDGE('',*,*,#4689,.F.);
#6132=ORIENTED_EDGE('',*,*,#4693,.F.);
#6133=ORIENTED_EDGE('',*,*,#4696,.F.);
#6134=ORIENTED_EDGE('',*,*,#4699,.F.);
#6135=ORIENTED_EDGE('',*,*,#4702,.F.);
#6136=ORIENTED_EDGE('',*,*,#4705,.T.);
#6137=ORIENTED_EDGE('',*,*,#4706,.F.);
#6138=ORIENTED_EDGE('',*,*,#4705,.F.);
#6139=ORIENTED_EDGE('',*,*,#4707,.T.);
#6140=ORIENTED_EDGE('',*,*,#4708,.T.);
#6141=ORIENTED_EDGE('',*,*,#4707,.F.);
#6142=ORIENTED_EDGE('',*,*,#4708,.F.);
#6143=ORIENTED_EDGE('',*,*,#4709,.F.);
#6144=ORIENTED_EDGE('',*,*,#4710,.F.);
#6145=ORIENTED_EDGE('',*,*,#4711,.T.);
#6146=ORIENTED_EDGE('',*,*,#4709,.T.);
#6147=ORIENTED_EDGE('',*,*,#4711,.F.);
#6148=ORIENTED_EDGE('',*,*,#4712,.F.);
#6149=ORIENTED_EDGE('',*,*,#4713,.T.);
#6150=ORIENTED_EDGE('',*,*,#4710,.T.);
#6151=ORIENTED_EDGE('',*,*,#4713,.F.);
#6152=ORIENTED_EDGE('',*,*,#4714,.F.);
#6153=ORIENTED_EDGE('',*,*,#4715,.T.);
#6154=ORIENTED_EDGE('',*,*,#4712,.T.);
#6155=ORIENTED_EDGE('',*,*,#4715,.F.);
#6156=ORIENTED_EDGE('',*,*,#4714,.T.);
#6157=ORIENTED_EDGE('',*,*,#4716,.F.);
#6158=ORIENTED_EDGE('',*,*,#4717,.F.);
#6159=ORIENTED_EDGE('',*,*,#4718,.T.);
#6160=ORIENTED_EDGE('',*,*,#4716,.T.);
#6161=ORIENTED_EDGE('',*,*,#4718,.F.);
#6162=ORIENTED_EDGE('',*,*,#4706,.T.);
#6163=ORIENTED_EDGE('',*,*,#4719,.T.);
#6164=ORIENTED_EDGE('',*,*,#4717,.T.);
#6165=ORIENTED_EDGE('',*,*,#4719,.F.);
#6166=ORIENTED_EDGE('',*,*,#4720,.F.);
#6167=ORIENTED_EDGE('',*,*,#4721,.F.);
#6168=ORIENTED_EDGE('',*,*,#4722,.T.);
#6169=ORIENTED_EDGE('',*,*,#4720,.T.);
#6170=ORIENTED_EDGE('',*,*,#4722,.F.);
#6171=ORIENTED_EDGE('',*,*,#4723,.F.);
#6172=ORIENTED_EDGE('',*,*,#4724,.T.);
#6173=ORIENTED_EDGE('',*,*,#4721,.T.);
#6174=ORIENTED_EDGE('',*,*,#4724,.F.);
#6175=ORIENTED_EDGE('',*,*,#4725,.F.);
#6176=ORIENTED_EDGE('',*,*,#4726,.T.);
#6177=ORIENTED_EDGE('',*,*,#4723,.T.);
#6178=ORIENTED_EDGE('',*,*,#4726,.F.);
#6179=ORIENTED_EDGE('',*,*,#4725,.T.);
#6180=ORIENTED_EDGE('',*,*,#4727,.F.);
#6181=ORIENTED_EDGE('',*,*,#4728,.F.);
#6182=ORIENTED_EDGE('',*,*,#4729,.T.);
#6183=ORIENTED_EDGE('',*,*,#4727,.T.);
#6184=ORIENTED_EDGE('',*,*,#4729,.F.);
#6185=ORIENTED_EDGE('',*,*,#4730,.F.);
#6186=ORIENTED_EDGE('',*,*,#4731,.T.);
#6187=ORIENTED_EDGE('',*,*,#4728,.T.);
#6188=ORIENTED_EDGE('',*,*,#4731,.F.);
#6189=ORIENTED_EDGE('',*,*,#4732,.F.);
#6190=ORIENTED_EDGE('',*,*,#4733,.T.);
#6191=ORIENTED_EDGE('',*,*,#4730,.T.);
#6192=ORIENTED_EDGE('',*,*,#4733,.F.);
#6193=ORIENTED_EDGE('',*,*,#4732,.T.);
#6194=ORIENTED_EDGE('',*,*,#4734,.T.);
#6195=ORIENTED_EDGE('',*,*,#4735,.T.);
#6196=ORIENTED_EDGE('',*,*,#4736,.T.);
#6197=ORIENTED_EDGE('',*,*,#4737,.F.);
#6198=ORIENTED_EDGE('',*,*,#4738,.T.);
#6199=ORIENTED_EDGE('',*,*,#4739,.T.);
#6200=ORIENTED_EDGE('',*,*,#4740,.T.);
#6201=ORIENTED_EDGE('',*,*,#4735,.F.);
#6202=ORIENTED_EDGE('',*,*,#4741,.T.);
#6203=ORIENTED_EDGE('',*,*,#4742,.T.);
#6204=ORIENTED_EDGE('',*,*,#4743,.T.);
#6205=ORIENTED_EDGE('',*,*,#4739,.F.);
#6206=ORIENTED_EDGE('',*,*,#4744,.T.);
#6207=ORIENTED_EDGE('',*,*,#4745,.T.);
#6208=ORIENTED_EDGE('',*,*,#4746,.T.);
#6209=ORIENTED_EDGE('',*,*,#4742,.F.);
#6210=ORIENTED_EDGE('',*,*,#4747,.T.);
#6211=ORIENTED_EDGE('',*,*,#4748,.T.);
#6212=ORIENTED_EDGE('',*,*,#4749,.T.);
#6213=ORIENTED_EDGE('',*,*,#4745,.F.);
#6214=ORIENTED_EDGE('',*,*,#4750,.T.);
#6215=ORIENTED_EDGE('',*,*,#4737,.T.);
#6216=ORIENTED_EDGE('',*,*,#4751,.T.);
#6217=ORIENTED_EDGE('',*,*,#4748,.F.);
#6218=ORIENTED_EDGE('',*,*,#4750,.F.);
#6219=ORIENTED_EDGE('',*,*,#4747,.F.);
#6220=ORIENTED_EDGE('',*,*,#4744,.F.);
#6221=ORIENTED_EDGE('',*,*,#4741,.F.);
#6222=ORIENTED_EDGE('',*,*,#4738,.F.);
#6223=ORIENTED_EDGE('',*,*,#4734,.F.);
#6224=ORIENTED_EDGE('',*,*,#4751,.F.);
#6225=ORIENTED_EDGE('',*,*,#4736,.F.);
#6226=ORIENTED_EDGE('',*,*,#4740,.F.);
#6227=ORIENTED_EDGE('',*,*,#4743,.F.);
#6228=ORIENTED_EDGE('',*,*,#4746,.F.);
#6229=ORIENTED_EDGE('',*,*,#4749,.F.);
#6230=ORIENTED_EDGE('',*,*,#4752,.F.);
#6231=ORIENTED_EDGE('',*,*,#4753,.T.);
#6232=ORIENTED_EDGE('',*,*,#4754,.F.);
#6233=ORIENTED_EDGE('',*,*,#4753,.F.);
#6234=ORIENTED_EDGE('',*,*,#4755,.F.);
#6235=ORIENTED_EDGE('',*,*,#4756,.T.);
#6236=ORIENTED_EDGE('',*,*,#4757,.F.);
#6237=ORIENTED_EDGE('',*,*,#4756,.F.);
#6238=ORIENTED_EDGE('',*,*,#4758,.F.);
#6239=ORIENTED_EDGE('',*,*,#4759,.T.);
#6240=ORIENTED_EDGE('',*,*,#4760,.F.);
#6241=ORIENTED_EDGE('',*,*,#4759,.F.);
#6242=ORIENTED_EDGE('',*,*,#4761,.F.);
#6243=ORIENTED_EDGE('',*,*,#4762,.T.);
#6244=ORIENTED_EDGE('',*,*,#4763,.F.);
#6245=ORIENTED_EDGE('',*,*,#4762,.F.);
#6246=ORIENTED_EDGE('',*,*,#4764,.T.);
#6247=ORIENTED_EDGE('',*,*,#4765,.T.);
#6248=ORIENTED_EDGE('',*,*,#4766,.F.);
#6249=ORIENTED_EDGE('',*,*,#4767,.F.);
#6250=ORIENTED_EDGE('',*,*,#4754,.T.);
#6251=ORIENTED_EDGE('',*,*,#4757,.T.);
#6252=ORIENTED_EDGE('',*,*,#4760,.T.);
#6253=ORIENTED_EDGE('',*,*,#4763,.T.);
#6254=ORIENTED_EDGE('',*,*,#4768,.T.);
#6255=ORIENTED_EDGE('',*,*,#4767,.T.);
#6256=ORIENTED_EDGE('',*,*,#4769,.F.);
#6257=ORIENTED_EDGE('',*,*,#4770,.F.);
#6258=ORIENTED_EDGE('',*,*,#4771,.T.);
#6259=ORIENTED_EDGE('',*,*,#4770,.T.);
#6260=ORIENTED_EDGE('',*,*,#4772,.F.);
#6261=ORIENTED_EDGE('',*,*,#4773,.F.);
#6262=ORIENTED_EDGE('',*,*,#4752,.T.);
#6263=ORIENTED_EDGE('',*,*,#4755,.T.);
#6264=ORIENTED_EDGE('',*,*,#4758,.T.);
#6265=ORIENTED_EDGE('',*,*,#4761,.T.);
#6266=ORIENTED_EDGE('',*,*,#4774,.T.);
#6267=ORIENTED_EDGE('',*,*,#4773,.T.);
#6268=ORIENTED_EDGE('',*,*,#4775,.F.);
#6269=ORIENTED_EDGE('',*,*,#4765,.F.);
#6270=ORIENTED_EDGE('',*,*,#4775,.T.);
#6271=ORIENTED_EDGE('',*,*,#4772,.T.);
#6272=ORIENTED_EDGE('',*,*,#4769,.T.);
#6273=ORIENTED_EDGE('',*,*,#4766,.T.);
#6274=ORIENTED_EDGE('',*,*,#4774,.F.);
#6275=ORIENTED_EDGE('',*,*,#4764,.F.);
#6276=ORIENTED_EDGE('',*,*,#4768,.F.);
#6277=ORIENTED_EDGE('',*,*,#4771,.F.);
#6278=ORIENTED_EDGE('',*,*,#4776,.T.);
#6279=ORIENTED_EDGE('',*,*,#4777,.T.);
#6280=ORIENTED_EDGE('',*,*,#4778,.T.);
#6281=ORIENTED_EDGE('',*,*,#4777,.F.);
#6282=ORIENTED_EDGE('',*,*,#4778,.F.);
#6283=ORIENTED_EDGE('',*,*,#4779,.T.);
#6284=ORIENTED_EDGE('',*,*,#4780,.T.);
#6285=ORIENTED_EDGE('',*,*,#4779,.F.);
#6286=ORIENTED_EDGE('',*,*,#4781,.T.);
#6287=ORIENTED_EDGE('',*,*,#4776,.F.);
#6288=ORIENTED_EDGE('',*,*,#4781,.F.);
#6289=ORIENTED_EDGE('',*,*,#4782,.T.);
#6290=ORIENTED_EDGE('',*,*,#4783,.T.);
#6291=ORIENTED_EDGE('',*,*,#4782,.F.);
#6292=ORIENTED_EDGE('',*,*,#4783,.F.);
#6293=ORIENTED_EDGE('',*,*,#4780,.F.);
#6294=ORIENTED_EDGE('',*,*,#4784,.F.);
#6295=ORIENTED_EDGE('',*,*,#4785,.T.);
#6296=ORIENTED_EDGE('',*,*,#4786,.F.);
#6297=ORIENTED_EDGE('',*,*,#4785,.F.);
#6298=ORIENTED_EDGE('',*,*,#4787,.F.);
#6299=ORIENTED_EDGE('',*,*,#4788,.T.);
#6300=ORIENTED_EDGE('',*,*,#4789,.F.);
#6301=ORIENTED_EDGE('',*,*,#4788,.F.);
#6302=ORIENTED_EDGE('',*,*,#4790,.T.);
#6303=ORIENTED_EDGE('',*,*,#4791,.T.);
#6304=ORIENTED_EDGE('',*,*,#4792,.F.);
#6305=ORIENTED_EDGE('',*,*,#4793,.F.);
#6306=ORIENTED_EDGE('',*,*,#4794,.T.);
#6307=ORIENTED_EDGE('',*,*,#4793,.T.);
#6308=ORIENTED_EDGE('',*,*,#4795,.F.);
#6309=ORIENTED_EDGE('',*,*,#4796,.F.);
#6310=ORIENTED_EDGE('',*,*,#4797,.T.);
#6311=ORIENTED_EDGE('',*,*,#4796,.T.);
#6312=ORIENTED_EDGE('',*,*,#4798,.F.);
#6313=ORIENTED_EDGE('',*,*,#4799,.F.);
#6314=ORIENTED_EDGE('',*,*,#4800,.T.);
#6315=ORIENTED_EDGE('',*,*,#4799,.T.);
#6316=ORIENTED_EDGE('',*,*,#4801,.F.);
#6317=ORIENTED_EDGE('',*,*,#4791,.F.);
#6318=ORIENTED_EDGE('',*,*,#4801,.T.);
#6319=ORIENTED_EDGE('',*,*,#4798,.T.);
#6320=ORIENTED_EDGE('',*,*,#4795,.T.);
#6321=ORIENTED_EDGE('',*,*,#4792,.T.);
#6322=ORIENTED_EDGE('',*,*,#4786,.T.);
#6323=ORIENTED_EDGE('',*,*,#4789,.T.);
#6324=ORIENTED_EDGE('',*,*,#4800,.F.);
#6325=ORIENTED_EDGE('',*,*,#4790,.F.);
#6326=ORIENTED_EDGE('',*,*,#4794,.F.);
#6327=ORIENTED_EDGE('',*,*,#4797,.F.);
#6328=ORIENTED_EDGE('',*,*,#4784,.T.);
#6329=ORIENTED_EDGE('',*,*,#4787,.T.);
#6330=ORIENTED_EDGE('',*,*,#4802,.T.);
#6331=ORIENTED_EDGE('',*,*,#4803,.T.);
#6332=ORIENTED_EDGE('',*,*,#4804,.F.);
#6333=ORIENTED_EDGE('',*,*,#4805,.F.);
#6334=ORIENTED_EDGE('',*,*,#4806,.T.);
#6335=ORIENTED_EDGE('',*,*,#4805,.T.);
#6336=ORIENTED_EDGE('',*,*,#4807,.F.);
#6337=ORIENTED_EDGE('',*,*,#4808,.F.);
#6338=ORIENTED_EDGE('',*,*,#4809,.T.);
#6339=ORIENTED_EDGE('',*,*,#4808,.T.);
#6340=ORIENTED_EDGE('',*,*,#4810,.F.);
#6341=ORIENTED_EDGE('',*,*,#4811,.F.);
#6342=ORIENTED_EDGE('',*,*,#4812,.T.);
#6343=ORIENTED_EDGE('',*,*,#4811,.T.);
#6344=ORIENTED_EDGE('',*,*,#4813,.F.);
#6345=ORIENTED_EDGE('',*,*,#4803,.F.);
#6346=ORIENTED_EDGE('',*,*,#4813,.T.);
#6347=ORIENTED_EDGE('',*,*,#4810,.T.);
#6348=ORIENTED_EDGE('',*,*,#4807,.T.);
#6349=ORIENTED_EDGE('',*,*,#4804,.T.);
#6350=ORIENTED_EDGE('',*,*,#4812,.F.);
#6351=ORIENTED_EDGE('',*,*,#4802,.F.);
#6352=ORIENTED_EDGE('',*,*,#4806,.F.);
#6353=ORIENTED_EDGE('',*,*,#4809,.F.);
#6354=ORIENTED_EDGE('',*,*,#4814,.T.);
#6355=ORIENTED_EDGE('',*,*,#4815,.T.);
#6356=ORIENTED_EDGE('',*,*,#4816,.F.);
#6357=ORIENTED_EDGE('',*,*,#4817,.F.);
#6358=ORIENTED_EDGE('',*,*,#4818,.T.);
#6359=ORIENTED_EDGE('',*,*,#4817,.T.);
#6360=ORIENTED_EDGE('',*,*,#4819,.F.);
#6361=ORIENTED_EDGE('',*,*,#4820,.F.);
#6362=ORIENTED_EDGE('',*,*,#4821,.T.);
#6363=ORIENTED_EDGE('',*,*,#4820,.T.);
#6364=ORIENTED_EDGE('',*,*,#4822,.F.);
#6365=ORIENTED_EDGE('',*,*,#4823,.F.);
#6366=ORIENTED_EDGE('',*,*,#4824,.T.);
#6367=ORIENTED_EDGE('',*,*,#4823,.T.);
#6368=ORIENTED_EDGE('',*,*,#4825,.F.);
#6369=ORIENTED_EDGE('',*,*,#4815,.F.);
#6370=ORIENTED_EDGE('',*,*,#4825,.T.);
#6371=ORIENTED_EDGE('',*,*,#4822,.T.);
#6372=ORIENTED_EDGE('',*,*,#4819,.T.);
#6373=ORIENTED_EDGE('',*,*,#4816,.T.);
#6374=ORIENTED_EDGE('',*,*,#4824,.F.);
#6375=ORIENTED_EDGE('',*,*,#4814,.F.);
#6376=ORIENTED_EDGE('',*,*,#4818,.F.);
#6377=ORIENTED_EDGE('',*,*,#4821,.F.);
#6378=ORIENTED_EDGE('',*,*,#4826,.F.);
#6379=ORIENTED_EDGE('',*,*,#4827,.T.);
#6380=ORIENTED_EDGE('',*,*,#4828,.F.);
#6381=ORIENTED_EDGE('',*,*,#4827,.F.);
#6382=ORIENTED_EDGE('',*,*,#4829,.F.);
#6383=ORIENTED_EDGE('',*,*,#4830,.T.);
#6384=ORIENTED_EDGE('',*,*,#4831,.F.);
#6385=ORIENTED_EDGE('',*,*,#4830,.F.);
#6386=ORIENTED_EDGE('',*,*,#4832,.T.);
#6387=ORIENTED_EDGE('',*,*,#4833,.T.);
#6388=ORIENTED_EDGE('',*,*,#4834,.F.);
#6389=ORIENTED_EDGE('',*,*,#4835,.F.);
#6390=ORIENTED_EDGE('',*,*,#4836,.T.);
#6391=ORIENTED_EDGE('',*,*,#4835,.T.);
#6392=ORIENTED_EDGE('',*,*,#4837,.F.);
#6393=ORIENTED_EDGE('',*,*,#4838,.F.);
#6394=ORIENTED_EDGE('',*,*,#4839,.T.);
#6395=ORIENTED_EDGE('',*,*,#4838,.T.);
#6396=ORIENTED_EDGE('',*,*,#4840,.F.);
#6397=ORIENTED_EDGE('',*,*,#4841,.F.);
#6398=ORIENTED_EDGE('',*,*,#4842,.T.);
#6399=ORIENTED_EDGE('',*,*,#4841,.T.);
#6400=ORIENTED_EDGE('',*,*,#4843,.F.);
#6401=ORIENTED_EDGE('',*,*,#4833,.F.);
#6402=ORIENTED_EDGE('',*,*,#4843,.T.);
#6403=ORIENTED_EDGE('',*,*,#4840,.T.);
#6404=ORIENTED_EDGE('',*,*,#4837,.T.);
#6405=ORIENTED_EDGE('',*,*,#4834,.T.);
#6406=ORIENTED_EDGE('',*,*,#4828,.T.);
#6407=ORIENTED_EDGE('',*,*,#4831,.T.);
#6408=ORIENTED_EDGE('',*,*,#4842,.F.);
#6409=ORIENTED_EDGE('',*,*,#4832,.F.);
#6410=ORIENTED_EDGE('',*,*,#4836,.F.);
#6411=ORIENTED_EDGE('',*,*,#4839,.F.);
#6412=ORIENTED_EDGE('',*,*,#4826,.T.);
#6413=ORIENTED_EDGE('',*,*,#4829,.T.);
#6414=ORIENTED_EDGE('',*,*,#4844,.T.);
#6415=ORIENTED_EDGE('',*,*,#4845,.T.);
#6416=ORIENTED_EDGE('',*,*,#4846,.F.);
#6417=ORIENTED_EDGE('',*,*,#4847,.F.);
#6418=ORIENTED_EDGE('',*,*,#4848,.T.);
#6419=ORIENTED_EDGE('',*,*,#4847,.T.);
#6420=ORIENTED_EDGE('',*,*,#4849,.F.);
#6421=ORIENTED_EDGE('',*,*,#4850,.F.);
#6422=ORIENTED_EDGE('',*,*,#4851,.T.);
#6423=ORIENTED_EDGE('',*,*,#4850,.T.);
#6424=ORIENTED_EDGE('',*,*,#4852,.F.);
#6425=ORIENTED_EDGE('',*,*,#4853,.F.);
#6426=ORIENTED_EDGE('',*,*,#4854,.T.);
#6427=ORIENTED_EDGE('',*,*,#4853,.T.);
#6428=ORIENTED_EDGE('',*,*,#4855,.F.);
#6429=ORIENTED_EDGE('',*,*,#4845,.F.);
#6430=ORIENTED_EDGE('',*,*,#4855,.T.);
#6431=ORIENTED_EDGE('',*,*,#4852,.T.);
#6432=ORIENTED_EDGE('',*,*,#4849,.T.);
#6433=ORIENTED_EDGE('',*,*,#4846,.T.);
#6434=ORIENTED_EDGE('',*,*,#4854,.F.);
#6435=ORIENTED_EDGE('',*,*,#4844,.F.);
#6436=ORIENTED_EDGE('',*,*,#4848,.F.);
#6437=ORIENTED_EDGE('',*,*,#4851,.F.);
#6438=ORIENTED_EDGE('',*,*,#4856,.T.);
#6439=ORIENTED_EDGE('',*,*,#4857,.T.);
#6440=ORIENTED_EDGE('',*,*,#4858,.F.);
#6441=ORIENTED_EDGE('',*,*,#4859,.F.);
#6442=ORIENTED_EDGE('',*,*,#4860,.T.);
#6443=ORIENTED_EDGE('',*,*,#4859,.T.);
#6444=ORIENTED_EDGE('',*,*,#4861,.F.);
#6445=ORIENTED_EDGE('',*,*,#4862,.F.);
#6446=ORIENTED_EDGE('',*,*,#4863,.T.);
#6447=ORIENTED_EDGE('',*,*,#4862,.T.);
#6448=ORIENTED_EDGE('',*,*,#4864,.F.);
#6449=ORIENTED_EDGE('',*,*,#4865,.F.);
#6450=ORIENTED_EDGE('',*,*,#4866,.T.);
#6451=ORIENTED_EDGE('',*,*,#4865,.T.);
#6452=ORIENTED_EDGE('',*,*,#4867,.F.);
#6453=ORIENTED_EDGE('',*,*,#4857,.F.);
#6454=ORIENTED_EDGE('',*,*,#4867,.T.);
#6455=ORIENTED_EDGE('',*,*,#4864,.T.);
#6456=ORIENTED_EDGE('',*,*,#4861,.T.);
#6457=ORIENTED_EDGE('',*,*,#4858,.T.);
#6458=ORIENTED_EDGE('',*,*,#4866,.F.);
#6459=ORIENTED_EDGE('',*,*,#4856,.F.);
#6460=ORIENTED_EDGE('',*,*,#4860,.F.);
#6461=ORIENTED_EDGE('',*,*,#4863,.F.);
#6462=ORIENTED_EDGE('',*,*,#4868,.F.);
#6463=ORIENTED_EDGE('',*,*,#4869,.T.);
#6464=ORIENTED_EDGE('',*,*,#4870,.T.);
#6465=ORIENTED_EDGE('',*,*,#4869,.F.);
#6466=ORIENTED_EDGE('',*,*,#4871,.F.);
#6467=ORIENTED_EDGE('',*,*,#4872,.T.);
#6468=ORIENTED_EDGE('',*,*,#4873,.T.);
#6469=ORIENTED_EDGE('',*,*,#4872,.F.);
#6470=ORIENTED_EDGE('',*,*,#4871,.T.);
#6471=ORIENTED_EDGE('',*,*,#4868,.T.);
#6472=ORIENTED_EDGE('',*,*,#4873,.F.);
#6473=ORIENTED_EDGE('',*,*,#4870,.F.);
#6474=ORIENTED_EDGE('',*,*,#4874,.F.);
#6475=ORIENTED_EDGE('',*,*,#4875,.T.);
#6476=ORIENTED_EDGE('',*,*,#4876,.T.);
#6477=ORIENTED_EDGE('',*,*,#4875,.F.);
#6478=ORIENTED_EDGE('',*,*,#4877,.F.);
#6479=ORIENTED_EDGE('',*,*,#4876,.F.);
#6480=ORIENTED_EDGE('',*,*,#4877,.T.);
#6481=ORIENTED_EDGE('',*,*,#4878,.T.);
#6482=ORIENTED_EDGE('',*,*,#4879,.T.);
#6483=ORIENTED_EDGE('',*,*,#4878,.F.);
#6484=ORIENTED_EDGE('',*,*,#4880,.F.);
#6485=ORIENTED_EDGE('',*,*,#4881,.T.);
#6486=ORIENTED_EDGE('',*,*,#4882,.T.);
#6487=ORIENTED_EDGE('',*,*,#4881,.F.);
#6488=ORIENTED_EDGE('',*,*,#4880,.T.);
#6489=ORIENTED_EDGE('',*,*,#4874,.T.);
#6490=ORIENTED_EDGE('',*,*,#4882,.F.);
#6491=ORIENTED_EDGE('',*,*,#4879,.F.);
#6492=ORIENTED_EDGE('',*,*,#4883,.F.);
#6493=ORIENTED_EDGE('',*,*,#4884,.T.);
#6494=ORIENTED_EDGE('',*,*,#4885,.F.);
#6495=ORIENTED_EDGE('',*,*,#4884,.F.);
#6496=ORIENTED_EDGE('',*,*,#4885,.T.);
#6497=ORIENTED_EDGE('',*,*,#4886,.T.);
#6498=ORIENTED_EDGE('',*,*,#4886,.F.);
#6499=ORIENTED_EDGE('',*,*,#4887,.T.);
#6500=ORIENTED_EDGE('',*,*,#4888,.T.);
#6501=ORIENTED_EDGE('',*,*,#4887,.F.);
#6502=ORIENTED_EDGE('',*,*,#4889,.F.);
#6503=ORIENTED_EDGE('',*,*,#4890,.T.);
#6504=ORIENTED_EDGE('',*,*,#4891,.T.);
#6505=ORIENTED_EDGE('',*,*,#4890,.F.);
#6506=ORIENTED_EDGE('',*,*,#4889,.T.);
#6507=ORIENTED_EDGE('',*,*,#4883,.T.);
#6508=ORIENTED_EDGE('',*,*,#4891,.F.);
#6509=ORIENTED_EDGE('',*,*,#4888,.F.);
#6510=ORIENTED_EDGE('',*,*,#4892,.F.);
#6511=ORIENTED_EDGE('',*,*,#4893,.T.);
#6512=ORIENTED_EDGE('',*,*,#4894,.T.);
#6513=ORIENTED_EDGE('',*,*,#4893,.F.);
#6514=ORIENTED_EDGE('',*,*,#4895,.F.);
#6515=ORIENTED_EDGE('',*,*,#4892,.T.);
#6516=ORIENTED_EDGE('',*,*,#4896,.F.);
#6517=ORIENTED_EDGE('',*,*,#4897,.T.);
#6518=ORIENTED_EDGE('',*,*,#4895,.T.);
#6519=ORIENTED_EDGE('',*,*,#4897,.F.);
#6520=ORIENTED_EDGE('',*,*,#4898,.F.);
#6521=ORIENTED_EDGE('',*,*,#4899,.T.);
#6522=ORIENTED_EDGE('',*,*,#4900,.T.);
#6523=ORIENTED_EDGE('',*,*,#4899,.F.);
#6524=ORIENTED_EDGE('',*,*,#4898,.T.);
#6525=ORIENTED_EDGE('',*,*,#4896,.T.);
#6526=ORIENTED_EDGE('',*,*,#4900,.F.);
#6527=ORIENTED_EDGE('',*,*,#4894,.F.);
#6528=ORIENTED_EDGE('',*,*,#4901,.F.);
#6529=ORIENTED_EDGE('',*,*,#4902,.T.);
#6530=ORIENTED_EDGE('',*,*,#4903,.T.);
#6531=ORIENTED_EDGE('',*,*,#4902,.F.);
#6532=ORIENTED_EDGE('',*,*,#4901,.T.);
#6533=ORIENTED_EDGE('',*,*,#4904,.F.);
#6534=ORIENTED_EDGE('',*,*,#4905,.F.);
#6535=ORIENTED_EDGE('',*,*,#4906,.T.);
#6536=ORIENTED_EDGE('',*,*,#4904,.T.);
#6537=ORIENTED_EDGE('',*,*,#4906,.F.);
#6538=ORIENTED_EDGE('',*,*,#4907,.F.);
#6539=ORIENTED_EDGE('',*,*,#4908,.T.);
#6540=ORIENTED_EDGE('',*,*,#4909,.T.);
#6541=ORIENTED_EDGE('',*,*,#4908,.F.);
#6542=ORIENTED_EDGE('',*,*,#4907,.T.);
#6543=ORIENTED_EDGE('',*,*,#4905,.T.);
#6544=ORIENTED_EDGE('',*,*,#4909,.F.);
#6545=ORIENTED_EDGE('',*,*,#4903,.F.);
#6546=ORIENTED_EDGE('',*,*,#4910,.F.);
#6547=ORIENTED_EDGE('',*,*,#4911,.T.);
#6548=ORIENTED_EDGE('',*,*,#4912,.F.);
#6549=ORIENTED_EDGE('',*,*,#4911,.F.);
#6550=ORIENTED_EDGE('',*,*,#4910,.T.);
#6551=ORIENTED_EDGE('',*,*,#4913,.F.);
#6552=ORIENTED_EDGE('',*,*,#4914,.T.);
#6553=ORIENTED_EDGE('',*,*,#4915,.T.);
#6554=ORIENTED_EDGE('',*,*,#4914,.F.);
#6555=ORIENTED_EDGE('',*,*,#4915,.F.);
#6556=ORIENTED_EDGE('',*,*,#4916,.F.);
#6557=ORIENTED_EDGE('',*,*,#4917,.T.);
#6558=ORIENTED_EDGE('',*,*,#4918,.T.);
#6559=ORIENTED_EDGE('',*,*,#4917,.F.);
#6560=ORIENTED_EDGE('',*,*,#4916,.T.);
#6561=ORIENTED_EDGE('',*,*,#4912,.T.);
#6562=ORIENTED_EDGE('',*,*,#4918,.F.);
#6563=ORIENTED_EDGE('',*,*,#4913,.T.);
#6564=ORIENTED_EDGE('',*,*,#4919,.F.);
#6565=ORIENTED_EDGE('',*,*,#4920,.T.);
#6566=ORIENTED_EDGE('',*,*,#4921,.F.);
#6567=ORIENTED_EDGE('',*,*,#4920,.F.);
#6568=ORIENTED_EDGE('',*,*,#4919,.T.);
#6569=ORIENTED_EDGE('',*,*,#4922,.F.);
#6570=ORIENTED_EDGE('',*,*,#4923,.F.);
#6571=ORIENTED_EDGE('',*,*,#4924,.T.);
#6572=ORIENTED_EDGE('',*,*,#4925,.F.);
#6573=ORIENTED_EDGE('',*,*,#4924,.F.);
#6574=ORIENTED_EDGE('',*,*,#4923,.T.);
#6575=ORIENTED_EDGE('',*,*,#4926,.F.);
#6576=ORIENTED_EDGE('',*,*,#4927,.F.);
#6577=ORIENTED_EDGE('',*,*,#4928,.T.);
#6578=ORIENTED_EDGE('',*,*,#4922,.T.);
#6579=ORIENTED_EDGE('',*,*,#4928,.F.);
#6580=ORIENTED_EDGE('',*,*,#4929,.F.);
#6581=ORIENTED_EDGE('',*,*,#4930,.T.);
#6582=ORIENTED_EDGE('',*,*,#4926,.T.);
#6583=ORIENTED_EDGE('',*,*,#4930,.F.);
#6584=ORIENTED_EDGE('',*,*,#4931,.F.);
#6585=ORIENTED_EDGE('',*,*,#4932,.T.);
#6586=ORIENTED_EDGE('',*,*,#4933,.F.);
#6587=ORIENTED_EDGE('',*,*,#4932,.F.);
#6588=ORIENTED_EDGE('',*,*,#4934,.T.);
#6589=ORIENTED_EDGE('',*,*,#4935,.T.);
#6590=ORIENTED_EDGE('',*,*,#4936,.F.);
#6591=ORIENTED_EDGE('',*,*,#4937,.F.);
#6592=ORIENTED_EDGE('',*,*,#4933,.T.);
#6593=ORIENTED_EDGE('',*,*,#4938,.T.);
#6594=ORIENTED_EDGE('',*,*,#4937,.T.);
#6595=ORIENTED_EDGE('',*,*,#4939,.F.);
#6596=ORIENTED_EDGE('',*,*,#4940,.F.);
#6597=ORIENTED_EDGE('',*,*,#4941,.T.);
#6598=ORIENTED_EDGE('',*,*,#4940,.T.);
#6599=ORIENTED_EDGE('',*,*,#4942,.F.);
#6600=ORIENTED_EDGE('',*,*,#4943,.F.);
#6601=ORIENTED_EDGE('',*,*,#4931,.T.);
#6602=ORIENTED_EDGE('',*,*,#4944,.T.);
#6603=ORIENTED_EDGE('',*,*,#4943,.T.);
#6604=ORIENTED_EDGE('',*,*,#4945,.F.);
#6605=ORIENTED_EDGE('',*,*,#4935,.F.);
#6606=ORIENTED_EDGE('',*,*,#4945,.T.);
#6607=ORIENTED_EDGE('',*,*,#4942,.T.);
#6608=ORIENTED_EDGE('',*,*,#4939,.T.);
#6609=ORIENTED_EDGE('',*,*,#4936,.T.);
#6610=ORIENTED_EDGE('',*,*,#4921,.T.);
#6611=ORIENTED_EDGE('',*,*,#4925,.T.);
#6612=ORIENTED_EDGE('',*,*,#4944,.F.);
#6613=ORIENTED_EDGE('',*,*,#4934,.F.);
#6614=ORIENTED_EDGE('',*,*,#4938,.F.);
#6615=ORIENTED_EDGE('',*,*,#4941,.F.);
#6616=ORIENTED_EDGE('',*,*,#4927,.T.);
#6617=ORIENTED_EDGE('',*,*,#4929,.T.);
#6618=ORIENTED_EDGE('',*,*,#4946,.F.);
#6619=ORIENTED_EDGE('',*,*,#4947,.T.);
#6620=ORIENTED_EDGE('',*,*,#4948,.T.);
#6621=ORIENTED_EDGE('',*,*,#4947,.F.);
#6622=ORIENTED_EDGE('',*,*,#4949,.F.);
#6623=ORIENTED_EDGE('',*,*,#4950,.T.);
#6624=ORIENTED_EDGE('',*,*,#4951,.T.);
#6625=ORIENTED_EDGE('',*,*,#4950,.F.);
#6626=ORIENTED_EDGE('',*,*,#4949,.T.);
#6627=ORIENTED_EDGE('',*,*,#4946,.T.);
#6628=ORIENTED_EDGE('',*,*,#4951,.F.);
#6629=ORIENTED_EDGE('',*,*,#4948,.F.);
#6630=ORIENTED_EDGE('',*,*,#4952,.F.);
#6631=ORIENTED_EDGE('',*,*,#4953,.T.);
#6632=ORIENTED_EDGE('',*,*,#4954,.T.);
#6633=ORIENTED_EDGE('',*,*,#4953,.F.);
#6634=ORIENTED_EDGE('',*,*,#4955,.F.);
#6635=ORIENTED_EDGE('',*,*,#4956,.T.);
#6636=ORIENTED_EDGE('',*,*,#4957,.T.);
#6637=ORIENTED_EDGE('',*,*,#4956,.F.);
#6638=ORIENTED_EDGE('',*,*,#4955,.T.);
#6639=ORIENTED_EDGE('',*,*,#4952,.T.);
#6640=ORIENTED_EDGE('',*,*,#4957,.F.);
#6641=ORIENTED_EDGE('',*,*,#4954,.F.);
#6642=ORIENTED_EDGE('',*,*,#4958,.F.);
#6643=ORIENTED_EDGE('',*,*,#4959,.F.);
#6644=ORIENTED_EDGE('',*,*,#4960,.T.);
#6645=ORIENTED_EDGE('',*,*,#4961,.F.);
#6646=ORIENTED_EDGE('',*,*,#4962,.F.);
#6647=ORIENTED_EDGE('',*,*,#4960,.F.);
#6648=ORIENTED_EDGE('',*,*,#4961,.T.);
#6649=ORIENTED_EDGE('',*,*,#4962,.T.);
#6650=ORIENTED_EDGE('',*,*,#4963,.T.);
#6651=ORIENTED_EDGE('',*,*,#4964,.T.);
#6652=ORIENTED_EDGE('',*,*,#4963,.F.);
#6653=ORIENTED_EDGE('',*,*,#4965,.T.);
#6654=ORIENTED_EDGE('',*,*,#4966,.T.);
#6655=ORIENTED_EDGE('',*,*,#4967,.F.);
#6656=ORIENTED_EDGE('',*,*,#4966,.F.);
#6657=ORIENTED_EDGE('',*,*,#4967,.T.);
#6658=ORIENTED_EDGE('',*,*,#4968,.T.);
#6659=ORIENTED_EDGE('',*,*,#4969,.F.);
#6660=ORIENTED_EDGE('',*,*,#4968,.F.);
#6661=ORIENTED_EDGE('',*,*,#4964,.F.);
#6662=ORIENTED_EDGE('',*,*,#4969,.T.);
#6663=ORIENTED_EDGE('',*,*,#4970,.F.);
#6664=ORIENTED_EDGE('',*,*,#4971,.T.);
#6665=ORIENTED_EDGE('',*,*,#4958,.T.);
#6666=ORIENTED_EDGE('',*,*,#4959,.T.);
#6667=ORIENTED_EDGE('',*,*,#4971,.F.);
#6668=ORIENTED_EDGE('',*,*,#4970,.T.);
#6669=ORIENTED_EDGE('',*,*,#4972,.F.);
#6670=ORIENTED_EDGE('',*,*,#4972,.T.);
#6671=ORIENTED_EDGE('',*,*,#4973,.T.);
#6672=ORIENTED_EDGE('',*,*,#4965,.F.);
#6673=ORIENTED_EDGE('',*,*,#4973,.F.);
#6674=ORIENTED_EDGE('',*,*,#4974,.F.);
#6675=ORIENTED_EDGE('',*,*,#4975,.F.);
#6676=ORIENTED_EDGE('',*,*,#4976,.T.);
#6677=ORIENTED_EDGE('',*,*,#4977,.F.);
#6678=ORIENTED_EDGE('',*,*,#4978,.F.);
#6679=ORIENTED_EDGE('',*,*,#4976,.F.);
#6680=ORIENTED_EDGE('',*,*,#4979,.T.);
#6681=ORIENTED_EDGE('',*,*,#4980,.T.);
#6682=ORIENTED_EDGE('',*,*,#4977,.T.);
#6683=ORIENTED_EDGE('',*,*,#4978,.T.);
#6684=ORIENTED_EDGE('',*,*,#4980,.F.);
#6685=ORIENTED_EDGE('',*,*,#4981,.F.);
#6686=ORIENTED_EDGE('',*,*,#4982,.T.);
#6687=ORIENTED_EDGE('',*,*,#4983,.F.);
#6688=ORIENTED_EDGE('',*,*,#4984,.T.);
#6689=ORIENTED_EDGE('',*,*,#4981,.T.);
#6690=ORIENTED_EDGE('',*,*,#4984,.F.);
#6691=ORIENTED_EDGE('',*,*,#4985,.F.);
#6692=ORIENTED_EDGE('',*,*,#4986,.T.);
#6693=ORIENTED_EDGE('',*,*,#4983,.T.);
#6694=ORIENTED_EDGE('',*,*,#4986,.F.);
#6695=ORIENTED_EDGE('',*,*,#4987,.F.);
#6696=ORIENTED_EDGE('',*,*,#4988,.T.);
#6697=ORIENTED_EDGE('',*,*,#4985,.T.);
#6698=ORIENTED_EDGE('',*,*,#4988,.F.);
#6699=ORIENTED_EDGE('',*,*,#4987,.T.);
#6700=ORIENTED_EDGE('',*,*,#4979,.F.);
#6701=ORIENTED_EDGE('',*,*,#4974,.T.);
#6702=ORIENTED_EDGE('',*,*,#4975,.T.);
#6703=ORIENTED_EDGE('',*,*,#4989,.T.);
#6704=ORIENTED_EDGE('',*,*,#4982,.F.);
#6705=ORIENTED_EDGE('',*,*,#4989,.F.);
#6706=ORIENTED_EDGE('',*,*,#4990,.T.);
#6707=ORIENTED_EDGE('',*,*,#4990,.F.);
#6708=ORIENTED_EDGE('',*,*,#4991,.T.);
#6709=ORIENTED_EDGE('',*,*,#4991,.F.);
#6710=ORIENTED_EDGE('',*,*,#4992,.T.);
#6711=ORIENTED_EDGE('',*,*,#4992,.F.);
#6712=ORIENTED_EDGE('',*,*,#4993,.T.);
#6713=ORIENTED_EDGE('',*,*,#4993,.F.);
#6714=ORIENTED_EDGE('',*,*,#4994,.T.);
#6715=ORIENTED_EDGE('',*,*,#4994,.F.);
#6716=ORIENTED_EDGE('',*,*,#4995,.T.);
#6717=ORIENTED_EDGE('',*,*,#4995,.F.);
#6718=ORIENTED_EDGE('',*,*,#4996,.T.);
#6719=ORIENTED_EDGE('',*,*,#4996,.F.);
#6720=ORIENTED_EDGE('',*,*,#4997,.T.);
#6721=ORIENTED_EDGE('',*,*,#4997,.F.);
#6722=ORIENTED_EDGE('',*,*,#4998,.F.);
#6723=ORIENTED_EDGE('',*,*,#4999,.F.);
#6724=ORIENTED_EDGE('',*,*,#5000,.F.);
#6725=ORIENTED_EDGE('',*,*,#5001,.F.);
#6726=ORIENTED_EDGE('',*,*,#5000,.T.);
#6727=ORIENTED_EDGE('',*,*,#5002,.F.);
#6728=ORIENTED_EDGE('',*,*,#5003,.T.);
#6729=ORIENTED_EDGE('',*,*,#5004,.F.);
#6730=ORIENTED_EDGE('',*,*,#5005,.T.);
#6731=ORIENTED_EDGE('',*,*,#5006,.F.);
#6732=ORIENTED_EDGE('',*,*,#5007,.T.);
#6733=ORIENTED_EDGE('',*,*,#5008,.T.);
#6734=ORIENTED_EDGE('',*,*,#5009,.F.);
#6735=ORIENTED_EDGE('',*,*,#5008,.F.);
#6736=ORIENTED_EDGE('',*,*,#5010,.T.);
#6737=ORIENTED_EDGE('',*,*,#5011,.F.);
#6738=ORIENTED_EDGE('',*,*,#5012,.T.);
#6739=ORIENTED_EDGE('',*,*,#5013,.F.);
#6740=ORIENTED_EDGE('',*,*,#5014,.T.);
#6741=ORIENTED_EDGE('',*,*,#5015,.F.);
#6742=ORIENTED_EDGE('',*,*,#5016,.T.);
#6743=ORIENTED_EDGE('',*,*,#5017,.F.);
#6744=ORIENTED_EDGE('',*,*,#5018,.T.);
#6745=ORIENTED_EDGE('',*,*,#5019,.F.);
#6746=ORIENTED_EDGE('',*,*,#4999,.T.);
#6747=ORIENTED_EDGE('',*,*,#5020,.T.);
#6748=ORIENTED_EDGE('',*,*,#5021,.T.);
#6749=ORIENTED_EDGE('',*,*,#5002,.T.);
#6750=ORIENTED_EDGE('',*,*,#5022,.F.);
#6751=ORIENTED_EDGE('',*,*,#5023,.F.);
#6752=ORIENTED_EDGE('',*,*,#5003,.F.);
#6753=ORIENTED_EDGE('',*,*,#5021,.F.);
#6754=ORIENTED_EDGE('',*,*,#5023,.T.);
#6755=ORIENTED_EDGE('',*,*,#5024,.T.);
#6756=ORIENTED_EDGE('',*,*,#5025,.T.);
#6757=ORIENTED_EDGE('',*,*,#5004,.T.);
#6758=ORIENTED_EDGE('',*,*,#5026,.F.);
#6759=ORIENTED_EDGE('',*,*,#5027,.F.);
#6760=ORIENTED_EDGE('',*,*,#5005,.F.);
#6761=ORIENTED_EDGE('',*,*,#5025,.F.);
#6762=ORIENTED_EDGE('',*,*,#5027,.T.);
#6763=ORIENTED_EDGE('',*,*,#5028,.T.);
#6764=ORIENTED_EDGE('',*,*,#5029,.T.);
#6765=ORIENTED_EDGE('',*,*,#5006,.T.);
#6766=ORIENTED_EDGE('',*,*,#5030,.F.);
#6767=ORIENTED_EDGE('',*,*,#5031,.F.);
#6768=ORIENTED_EDGE('',*,*,#5010,.F.);
#6769=ORIENTED_EDGE('',*,*,#5007,.F.);
#6770=ORIENTED_EDGE('',*,*,#5029,.F.);
#6771=ORIENTED_EDGE('',*,*,#5032,.F.);
#6772=ORIENTED_EDGE('',*,*,#5031,.T.);
#6773=ORIENTED_EDGE('',*,*,#5033,.T.);
#6774=ORIENTED_EDGE('',*,*,#5034,.T.);
#6775=ORIENTED_EDGE('',*,*,#5011,.T.);
#6776=ORIENTED_EDGE('',*,*,#5035,.F.);
#6777=ORIENTED_EDGE('',*,*,#5036,.F.);
#6778=ORIENTED_EDGE('',*,*,#5012,.F.);
#6779=ORIENTED_EDGE('',*,*,#5034,.F.);
#6780=ORIENTED_EDGE('',*,*,#5036,.T.);
#6781=ORIENTED_EDGE('',*,*,#5037,.T.);
#6782=ORIENTED_EDGE('',*,*,#5038,.T.);
#6783=ORIENTED_EDGE('',*,*,#5013,.T.);
#6784=ORIENTED_EDGE('',*,*,#5039,.F.);
#6785=ORIENTED_EDGE('',*,*,#5040,.F.);
#6786=ORIENTED_EDGE('',*,*,#5014,.F.);
#6787=ORIENTED_EDGE('',*,*,#5038,.F.);
#6788=ORIENTED_EDGE('',*,*,#5040,.T.);
#6789=ORIENTED_EDGE('',*,*,#5041,.T.);
#6790=ORIENTED_EDGE('',*,*,#5042,.T.);
#6791=ORIENTED_EDGE('',*,*,#5015,.T.);
#6792=ORIENTED_EDGE('',*,*,#5016,.F.);
#6793=ORIENTED_EDGE('',*,*,#5042,.F.);
#6794=ORIENTED_EDGE('',*,*,#5043,.F.);
#6795=ORIENTED_EDGE('',*,*,#5044,.F.);
#6796=ORIENTED_EDGE('',*,*,#5045,.F.);
#6797=ORIENTED_EDGE('',*,*,#5046,.T.);
#6798=ORIENTED_EDGE('',*,*,#5032,.T.);
#6799=ORIENTED_EDGE('',*,*,#5028,.F.);
#6800=ORIENTED_EDGE('',*,*,#5026,.T.);
#6801=ORIENTED_EDGE('',*,*,#5024,.F.);
#6802=ORIENTED_EDGE('',*,*,#5022,.T.);
#6803=ORIENTED_EDGE('',*,*,#5020,.F.);
#6804=ORIENTED_EDGE('',*,*,#4998,.T.);
#6805=ORIENTED_EDGE('',*,*,#5047,.F.);
#6806=ORIENTED_EDGE('',*,*,#5048,.T.);
#6807=ORIENTED_EDGE('',*,*,#5049,.F.);
#6808=ORIENTED_EDGE('',*,*,#5043,.T.);
#6809=ORIENTED_EDGE('',*,*,#5041,.F.);
#6810=ORIENTED_EDGE('',*,*,#5039,.T.);
#6811=ORIENTED_EDGE('',*,*,#5037,.F.);
#6812=ORIENTED_EDGE('',*,*,#5035,.T.);
#6813=ORIENTED_EDGE('',*,*,#5033,.F.);
#6814=ORIENTED_EDGE('',*,*,#5030,.T.);
#6815=ORIENTED_EDGE('',*,*,#5046,.F.);
#6816=ORIENTED_EDGE('',*,*,#5001,.T.);
#6817=ORIENTED_EDGE('',*,*,#5019,.T.);
#6818=ORIENTED_EDGE('',*,*,#5050,.T.);
#6819=ORIENTED_EDGE('',*,*,#5047,.T.);
#6820=ORIENTED_EDGE('',*,*,#5018,.F.);
#6821=ORIENTED_EDGE('',*,*,#5051,.F.);
#6822=ORIENTED_EDGE('',*,*,#5048,.F.);
#6823=ORIENTED_EDGE('',*,*,#5050,.F.);
#6824=ORIENTED_EDGE('',*,*,#5009,.T.);
#6825=ORIENTED_EDGE('',*,*,#5045,.T.);
#6826=ORIENTED_EDGE('',*,*,#5044,.T.);
#6827=ORIENTED_EDGE('',*,*,#5049,.T.);
#6828=ORIENTED_EDGE('',*,*,#5051,.T.);
#6829=ORIENTED_EDGE('',*,*,#5017,.T.);
#6830=ORIENTED_EDGE('',*,*,#5052,.F.);
#6831=ORIENTED_EDGE('',*,*,#5053,.T.);
#6832=ORIENTED_EDGE('',*,*,#5054,.F.);
#6833=ORIENTED_EDGE('',*,*,#5055,.T.);
#6834=ORIENTED_EDGE('',*,*,#5052,.T.);
#6835=ORIENTED_EDGE('',*,*,#5055,.F.);
#6836=ORIENTED_EDGE('',*,*,#5054,.T.);
#6837=ORIENTED_EDGE('',*,*,#5056,.F.);
#6838=ORIENTED_EDGE('',*,*,#5056,.T.);
#6839=ORIENTED_EDGE('',*,*,#5057,.T.);
#6840=ORIENTED_EDGE('',*,*,#5053,.F.);
#6841=ORIENTED_EDGE('',*,*,#5057,.F.);
#6842=ORIENTED_EDGE('',*,*,#5058,.F.);
#6843=ORIENTED_EDGE('',*,*,#5059,.T.);
#6844=ORIENTED_EDGE('',*,*,#5060,.F.);
#6845=ORIENTED_EDGE('',*,*,#5061,.T.);
#6846=ORIENTED_EDGE('',*,*,#5058,.T.);
#6847=ORIENTED_EDGE('',*,*,#5061,.F.);
#6848=ORIENTED_EDGE('',*,*,#5060,.T.);
#6849=ORIENTED_EDGE('',*,*,#5062,.F.);
#6850=ORIENTED_EDGE('',*,*,#5062,.T.);
#6851=ORIENTED_EDGE('',*,*,#5063,.T.);
#6852=ORIENTED_EDGE('',*,*,#5059,.F.);
#6853=ORIENTED_EDGE('',*,*,#5063,.F.);
#6854=ORIENTED_EDGE('',*,*,#5064,.F.);
#6855=ORIENTED_EDGE('',*,*,#5065,.T.);
#6856=ORIENTED_EDGE('',*,*,#5066,.T.);
#6857=ORIENTED_EDGE('',*,*,#5065,.F.);
#6858=ORIENTED_EDGE('',*,*,#5067,.F.);
#6859=ORIENTED_EDGE('',*,*,#5068,.T.);
#6860=ORIENTED_EDGE('',*,*,#5069,.T.);
#6861=ORIENTED_EDGE('',*,*,#5068,.F.);
#6862=ORIENTED_EDGE('',*,*,#5067,.T.);
#6863=ORIENTED_EDGE('',*,*,#5064,.T.);
#6864=ORIENTED_EDGE('',*,*,#5069,.F.);
#6865=ORIENTED_EDGE('',*,*,#5066,.F.);
#6866=ORIENTED_EDGE('',*,*,#5070,.T.);
#6867=ORIENTED_EDGE('',*,*,#5071,.T.);
#6868=ORIENTED_EDGE('',*,*,#5072,.T.);
#6869=ORIENTED_EDGE('',*,*,#5073,.F.);
#6870=ORIENTED_EDGE('',*,*,#5074,.T.);
#6871=ORIENTED_EDGE('',*,*,#5075,.T.);
#6872=ORIENTED_EDGE('',*,*,#5076,.T.);
#6873=ORIENTED_EDGE('',*,*,#5071,.F.);
#6874=ORIENTED_EDGE('',*,*,#5077,.T.);
#6875=ORIENTED_EDGE('',*,*,#5078,.T.);
#6876=ORIENTED_EDGE('',*,*,#5079,.T.);
#6877=ORIENTED_EDGE('',*,*,#5075,.F.);
#6878=ORIENTED_EDGE('',*,*,#5080,.T.);
#6879=ORIENTED_EDGE('',*,*,#5081,.T.);
#6880=ORIENTED_EDGE('',*,*,#5082,.T.);
#6881=ORIENTED_EDGE('',*,*,#5078,.F.);
#6882=ORIENTED_EDGE('',*,*,#5083,.T.);
#6883=ORIENTED_EDGE('',*,*,#5084,.T.);
#6884=ORIENTED_EDGE('',*,*,#5085,.T.);
#6885=ORIENTED_EDGE('',*,*,#5081,.F.);
#6886=ORIENTED_EDGE('',*,*,#5086,.T.);
#6887=ORIENTED_EDGE('',*,*,#5073,.T.);
#6888=ORIENTED_EDGE('',*,*,#5087,.T.);
#6889=ORIENTED_EDGE('',*,*,#5084,.F.);
#6890=ORIENTED_EDGE('',*,*,#5086,.F.);
#6891=ORIENTED_EDGE('',*,*,#5083,.F.);
#6892=ORIENTED_EDGE('',*,*,#5080,.F.);
#6893=ORIENTED_EDGE('',*,*,#5077,.F.);
#6894=ORIENTED_EDGE('',*,*,#5074,.F.);
#6895=ORIENTED_EDGE('',*,*,#5070,.F.);
#6896=ORIENTED_EDGE('',*,*,#5087,.F.);
#6897=ORIENTED_EDGE('',*,*,#5072,.F.);
#6898=ORIENTED_EDGE('',*,*,#5076,.F.);
#6899=ORIENTED_EDGE('',*,*,#5079,.F.);
#6900=ORIENTED_EDGE('',*,*,#5082,.F.);
#6901=ORIENTED_EDGE('',*,*,#5085,.F.);
#6902=ORIENTED_EDGE('',*,*,#5088,.F.);
#6903=ORIENTED_EDGE('',*,*,#5089,.F.);
#6904=ORIENTED_EDGE('',*,*,#5090,.F.);
#6905=ORIENTED_EDGE('',*,*,#5091,.T.);
#6906=ORIENTED_EDGE('',*,*,#5089,.T.);
#6907=ORIENTED_EDGE('',*,*,#5091,.F.);
#6908=ORIENTED_EDGE('',*,*,#5092,.F.);
#6909=ORIENTED_EDGE('',*,*,#5093,.T.);
#6910=ORIENTED_EDGE('',*,*,#5090,.T.);
#6911=ORIENTED_EDGE('',*,*,#5093,.F.);
#6912=ORIENTED_EDGE('',*,*,#5094,.F.);
#6913=ORIENTED_EDGE('',*,*,#5095,.T.);
#6914=ORIENTED_EDGE('',*,*,#5092,.T.);
#6915=ORIENTED_EDGE('',*,*,#5095,.F.);
#6916=ORIENTED_EDGE('',*,*,#5094,.T.);
#6917=ORIENTED_EDGE('',*,*,#5096,.F.);
#6918=ORIENTED_EDGE('',*,*,#5097,.F.);
#6919=ORIENTED_EDGE('',*,*,#5098,.T.);
#6920=ORIENTED_EDGE('',*,*,#5096,.T.);
#6921=ORIENTED_EDGE('',*,*,#5098,.F.);
#6922=ORIENTED_EDGE('',*,*,#5088,.T.);
#6923=ORIENTED_EDGE('',*,*,#5099,.T.);
#6924=ORIENTED_EDGE('',*,*,#5097,.T.);
#6925=ORIENTED_EDGE('',*,*,#5099,.F.);
#6926=ORIENTED_EDGE('',*,*,#5100,.F.);
#6927=ORIENTED_EDGE('',*,*,#5101,.T.);
#6928=ORIENTED_EDGE('',*,*,#5102,.T.);
#6929=ORIENTED_EDGE('',*,*,#5101,.F.);
#6930=ORIENTED_EDGE('',*,*,#5103,.F.);
#6931=ORIENTED_EDGE('',*,*,#5104,.T.);
#6932=ORIENTED_EDGE('',*,*,#5105,.T.);
#6933=ORIENTED_EDGE('',*,*,#5104,.F.);
#6934=ORIENTED_EDGE('',*,*,#5103,.T.);
#6935=ORIENTED_EDGE('',*,*,#5100,.T.);
#6936=ORIENTED_EDGE('',*,*,#5105,.F.);
#6937=ORIENTED_EDGE('',*,*,#5102,.F.);
#6938=ORIENTED_EDGE('',*,*,#5106,.F.);
#6939=ORIENTED_EDGE('',*,*,#5107,.F.);
#6940=ORIENTED_EDGE('',*,*,#5108,.F.);
#6941=ORIENTED_EDGE('',*,*,#5109,.F.);
#6942=ORIENTED_EDGE('',*,*,#5108,.T.);
#6943=ORIENTED_EDGE('',*,*,#5110,.T.);
#6944=ORIENTED_EDGE('',*,*,#5111,.F.);
#6945=ORIENTED_EDGE('',*,*,#5112,.F.);
#6946=ORIENTED_EDGE('',*,*,#5113,.T.);
#6947=ORIENTED_EDGE('',*,*,#5114,.T.);
#6948=ORIENTED_EDGE('',*,*,#5115,.T.);
#6949=ORIENTED_EDGE('',*,*,#5111,.T.);
#6950=ORIENTED_EDGE('',*,*,#5116,.T.);
#6951=ORIENTED_EDGE('',*,*,#5113,.F.);
#6952=ORIENTED_EDGE('',*,*,#5110,.F.);
#6953=ORIENTED_EDGE('',*,*,#5107,.T.);
#6954=ORIENTED_EDGE('',*,*,#5117,.F.);
#6955=ORIENTED_EDGE('',*,*,#5118,.F.);
#6956=ORIENTED_EDGE('',*,*,#5119,.T.);
#6957=ORIENTED_EDGE('',*,*,#5120,.F.);
#6958=ORIENTED_EDGE('',*,*,#5121,.T.);
#6959=ORIENTED_EDGE('',*,*,#5122,.T.);
#6960=ORIENTED_EDGE('',*,*,#5123,.T.);
#6961=ORIENTED_EDGE('',*,*,#5124,.T.);
#6962=ORIENTED_EDGE('',*,*,#5125,.T.);
#6963=ORIENTED_EDGE('',*,*,#5114,.F.);
#6964=ORIENTED_EDGE('',*,*,#5123,.F.);
#6965=ORIENTED_EDGE('',*,*,#5126,.F.);
#6966=ORIENTED_EDGE('',*,*,#5127,.F.);
#6967=ORIENTED_EDGE('',*,*,#5124,.F.);
#6968=ORIENTED_EDGE('',*,*,#5122,.F.);
#6969=ORIENTED_EDGE('',*,*,#5115,.F.);
#6970=ORIENTED_EDGE('',*,*,#5125,.F.);
#6971=ORIENTED_EDGE('',*,*,#5127,.T.);
#6972=ORIENTED_EDGE('',*,*,#5128,.F.);
#6973=ORIENTED_EDGE('',*,*,#5129,.F.);
#6974=ORIENTED_EDGE('',*,*,#5130,.T.);
#6975=ORIENTED_EDGE('',*,*,#5131,.F.);
#6976=ORIENTED_EDGE('',*,*,#5132,.T.);
#6977=ORIENTED_EDGE('',*,*,#5109,.T.);
#6978=ORIENTED_EDGE('',*,*,#5112,.T.);
#6979=ORIENTED_EDGE('',*,*,#5126,.T.);
#6980=ORIENTED_EDGE('',*,*,#5121,.F.);
#6981=ORIENTED_EDGE('',*,*,#5133,.F.);
#6982=ORIENTED_EDGE('',*,*,#5128,.T.);
#6983=ORIENTED_EDGE('',*,*,#5129,.T.);
#6984=ORIENTED_EDGE('',*,*,#5133,.T.);
#6985=ORIENTED_EDGE('',*,*,#5120,.T.);
#6986=ORIENTED_EDGE('',*,*,#5134,.T.);
#6987=ORIENTED_EDGE('',*,*,#5135,.T.);
#6988=ORIENTED_EDGE('',*,*,#5136,.T.);
#6989=ORIENTED_EDGE('',*,*,#5135,.F.);
#6990=ORIENTED_EDGE('',*,*,#5137,.F.);
#6991=ORIENTED_EDGE('',*,*,#5138,.T.);
#6992=ORIENTED_EDGE('',*,*,#5116,.F.);
#6993=ORIENTED_EDGE('',*,*,#5138,.F.);
#6994=ORIENTED_EDGE('',*,*,#5139,.F.);
#6995=ORIENTED_EDGE('',*,*,#5140,.F.);
#6996=ORIENTED_EDGE('',*,*,#5141,.F.);
#6997=ORIENTED_EDGE('',*,*,#5134,.F.);
#6998=ORIENTED_EDGE('',*,*,#5119,.F.);
#6999=ORIENTED_EDGE('',*,*,#5142,.F.);
#7000=ORIENTED_EDGE('',*,*,#5139,.T.);
#7001=ORIENTED_EDGE('',*,*,#5137,.T.);
#7002=ORIENTED_EDGE('',*,*,#5136,.F.);
#7003=ORIENTED_EDGE('',*,*,#5141,.T.);
#7004=ORIENTED_EDGE('',*,*,#5143,.F.);
#7005=ORIENTED_EDGE('',*,*,#5130,.F.);
#7006=ORIENTED_EDGE('',*,*,#5118,.T.);
#7007=ORIENTED_EDGE('',*,*,#5144,.T.);
#7008=ORIENTED_EDGE('',*,*,#5131,.T.);
#7009=ORIENTED_EDGE('',*,*,#5143,.T.);
#7010=ORIENTED_EDGE('',*,*,#5140,.T.);
#7011=ORIENTED_EDGE('',*,*,#5142,.T.);
#7012=ORIENTED_EDGE('',*,*,#5106,.T.);
#7013=ORIENTED_EDGE('',*,*,#5132,.F.);
#7014=ORIENTED_EDGE('',*,*,#5144,.F.);
#7015=ORIENTED_EDGE('',*,*,#5117,.T.);
#7016=ORIENTED_EDGE('',*,*,#5145,.T.);
#7017=ORIENTED_EDGE('',*,*,#5146,.T.);
#7018=ORIENTED_EDGE('',*,*,#5147,.T.);
#7019=ORIENTED_EDGE('',*,*,#5148,.F.);
#7020=ORIENTED_EDGE('',*,*,#5149,.T.);
#7021=ORIENTED_EDGE('',*,*,#5150,.T.);
#7022=ORIENTED_EDGE('',*,*,#5151,.T.);
#7023=ORIENTED_EDGE('',*,*,#5146,.F.);
#7024=ORIENTED_EDGE('',*,*,#5152,.T.);
#7025=ORIENTED_EDGE('',*,*,#5153,.T.);
#7026=ORIENTED_EDGE('',*,*,#5154,.T.);
#7027=ORIENTED_EDGE('',*,*,#5150,.F.);
#7028=ORIENTED_EDGE('',*,*,#5155,.T.);
#7029=ORIENTED_EDGE('',*,*,#5156,.T.);
#7030=ORIENTED_EDGE('',*,*,#5157,.T.);
#7031=ORIENTED_EDGE('',*,*,#5153,.F.);
#7032=ORIENTED_EDGE('',*,*,#5158,.T.);
#7033=ORIENTED_EDGE('',*,*,#5159,.T.);
#7034=ORIENTED_EDGE('',*,*,#5160,.T.);
#7035=ORIENTED_EDGE('',*,*,#5156,.F.);
#7036=ORIENTED_EDGE('',*,*,#5161,.T.);
#7037=ORIENTED_EDGE('',*,*,#5148,.T.);
#7038=ORIENTED_EDGE('',*,*,#5162,.T.);
#7039=ORIENTED_EDGE('',*,*,#5159,.F.);
#7040=ORIENTED_EDGE('',*,*,#5161,.F.);
#7041=ORIENTED_EDGE('',*,*,#5158,.F.);
#7042=ORIENTED_EDGE('',*,*,#5155,.F.);
#7043=ORIENTED_EDGE('',*,*,#5152,.F.);
#7044=ORIENTED_EDGE('',*,*,#5149,.F.);
#7045=ORIENTED_EDGE('',*,*,#5145,.F.);
#7046=ORIENTED_EDGE('',*,*,#5162,.F.);
#7047=ORIENTED_EDGE('',*,*,#5147,.F.);
#7048=ORIENTED_EDGE('',*,*,#5151,.F.);
#7049=ORIENTED_EDGE('',*,*,#5154,.F.);
#7050=ORIENTED_EDGE('',*,*,#5157,.F.);
#7051=ORIENTED_EDGE('',*,*,#5160,.F.);
#7052=ORIENTED_EDGE('',*,*,#5163,.F.);
#7053=ORIENTED_EDGE('',*,*,#5164,.F.);
#7054=ORIENTED_EDGE('',*,*,#5165,.F.);
#7055=ORIENTED_EDGE('',*,*,#5166,.T.);
#7056=ORIENTED_EDGE('',*,*,#5164,.T.);
#7057=ORIENTED_EDGE('',*,*,#5166,.F.);
#7058=ORIENTED_EDGE('',*,*,#5167,.F.);
#7059=ORIENTED_EDGE('',*,*,#5168,.T.);
#7060=ORIENTED_EDGE('',*,*,#5165,.T.);
#7061=ORIENTED_EDGE('',*,*,#5168,.F.);
#7062=ORIENTED_EDGE('',*,*,#5169,.F.);
#7063=ORIENTED_EDGE('',*,*,#5170,.T.);
#7064=ORIENTED_EDGE('',*,*,#5167,.T.);
#7065=ORIENTED_EDGE('',*,*,#5170,.F.);
#7066=ORIENTED_EDGE('',*,*,#5169,.T.);
#7067=ORIENTED_EDGE('',*,*,#5171,.F.);
#7068=ORIENTED_EDGE('',*,*,#5172,.F.);
#7069=ORIENTED_EDGE('',*,*,#5173,.T.);
#7070=ORIENTED_EDGE('',*,*,#5171,.T.);
#7071=ORIENTED_EDGE('',*,*,#5173,.F.);
#7072=ORIENTED_EDGE('',*,*,#5163,.T.);
#7073=ORIENTED_EDGE('',*,*,#5174,.T.);
#7074=ORIENTED_EDGE('',*,*,#5172,.T.);
#7075=ORIENTED_EDGE('',*,*,#5174,.F.);
#7076=ORIENTED_EDGE('',*,*,#5175,.F.);
#7077=ORIENTED_EDGE('',*,*,#5176,.T.);
#7078=ORIENTED_EDGE('',*,*,#5177,.F.);
#7079=ORIENTED_EDGE('',*,*,#5176,.F.);
#7080=ORIENTED_EDGE('',*,*,#5175,.T.);
#7081=ORIENTED_EDGE('',*,*,#5178,.F.);
#7082=ORIENTED_EDGE('',*,*,#5179,.F.);
#7083=ORIENTED_EDGE('',*,*,#5180,.T.);
#7084=ORIENTED_EDGE('',*,*,#5181,.F.);
#7085=ORIENTED_EDGE('',*,*,#5180,.F.);
#7086=ORIENTED_EDGE('',*,*,#5179,.T.);
#7087=ORIENTED_EDGE('',*,*,#5182,.F.);
#7088=ORIENTED_EDGE('',*,*,#5183,.F.);
#7089=ORIENTED_EDGE('',*,*,#5184,.T.);
#7090=ORIENTED_EDGE('',*,*,#5178,.T.);
#7091=ORIENTED_EDGE('',*,*,#5184,.F.);
#7092=ORIENTED_EDGE('',*,*,#5185,.F.);
#7093=ORIENTED_EDGE('',*,*,#5186,.T.);
#7094=ORIENTED_EDGE('',*,*,#5182,.T.);
#7095=ORIENTED_EDGE('',*,*,#5186,.F.);
#7096=ORIENTED_EDGE('',*,*,#5187,.F.);
#7097=ORIENTED_EDGE('',*,*,#5188,.T.);
#7098=ORIENTED_EDGE('',*,*,#5189,.F.);
#7099=ORIENTED_EDGE('',*,*,#5188,.F.);
#7100=ORIENTED_EDGE('',*,*,#5190,.T.);
#7101=ORIENTED_EDGE('',*,*,#5191,.T.);
#7102=ORIENTED_EDGE('',*,*,#5192,.F.);
#7103=ORIENTED_EDGE('',*,*,#5193,.F.);
#7104=ORIENTED_EDGE('',*,*,#5189,.T.);
#7105=ORIENTED_EDGE('',*,*,#5194,.T.);
#7106=ORIENTED_EDGE('',*,*,#5193,.T.);
#7107=ORIENTED_EDGE('',*,*,#5195,.F.);
#7108=ORIENTED_EDGE('',*,*,#5196,.F.);
#7109=ORIENTED_EDGE('',*,*,#5197,.T.);
#7110=ORIENTED_EDGE('',*,*,#5196,.T.);
#7111=ORIENTED_EDGE('',*,*,#5198,.F.);
#7112=ORIENTED_EDGE('',*,*,#5199,.F.);
#7113=ORIENTED_EDGE('',*,*,#5187,.T.);
#7114=ORIENTED_EDGE('',*,*,#5200,.T.);
#7115=ORIENTED_EDGE('',*,*,#5199,.T.);
#7116=ORIENTED_EDGE('',*,*,#5201,.F.);
#7117=ORIENTED_EDGE('',*,*,#5191,.F.);
#7118=ORIENTED_EDGE('',*,*,#5201,.T.);
#7119=ORIENTED_EDGE('',*,*,#5198,.T.);
#7120=ORIENTED_EDGE('',*,*,#5195,.T.);
#7121=ORIENTED_EDGE('',*,*,#5192,.T.);
#7122=ORIENTED_EDGE('',*,*,#5177,.T.);
#7123=ORIENTED_EDGE('',*,*,#5181,.T.);
#7124=ORIENTED_EDGE('',*,*,#5200,.F.);
#7125=ORIENTED_EDGE('',*,*,#5190,.F.);
#7126=ORIENTED_EDGE('',*,*,#5194,.F.);
#7127=ORIENTED_EDGE('',*,*,#5197,.F.);
#7128=ORIENTED_EDGE('',*,*,#5183,.T.);
#7129=ORIENTED_EDGE('',*,*,#5185,.T.);
#7130=CYLINDRICAL_SURFACE('',#8051,0.274999999999999);
#7131=CYLINDRICAL_SURFACE('',#8054,0.274999999999999);
#7132=CYLINDRICAL_SURFACE('',#8057,0.274999999999999);
#7133=CYLINDRICAL_SURFACE('',#8060,0.274999999999999);
#7134=CYLINDRICAL_SURFACE('',#8070,0.275);
#7135=CYLINDRICAL_SURFACE('',#8073,0.21);
#7136=CYLINDRICAL_SURFACE('',#8111,0.21);
#7137=CYLINDRICAL_SURFACE('',#8124,0.275);
#7138=CYLINDRICAL_SURFACE('',#8127,0.21);
#7139=CYLINDRICAL_SURFACE('',#8165,0.21);
#7140=CYLINDRICAL_SURFACE('',#8214,0.21);
#7141=CYLINDRICAL_SURFACE('',#8239,0.25);
#7142=CYLINDRICAL_SURFACE('',#8246,0.425);
#7143=CYLINDRICAL_SURFACE('',#8254,0.24505);
#7144=CYLINDRICAL_SURFACE('',#8260,0.425);
#7145=CYLINDRICAL_SURFACE('',#8268,0.24505);
#7146=CYLINDRICAL_SURFACE('',#8282,0.274999999999999);
#7147=CYLINDRICAL_SURFACE('',#8285,0.274999999999999);
#7148=CYLINDRICAL_SURFACE('',#8288,0.274999999999999);
#7149=CYLINDRICAL_SURFACE('',#8291,0.274999999999999);
#7150=CYLINDRICAL_SURFACE('',#8304,0.265);
#7151=CYLINDRICAL_SURFACE('',#8308,0.5);
#7152=CYLINDRICAL_SURFACE('',#8312,0.275);
#7153=CYLINDRICAL_SURFACE('',#8315,0.275);
#7154=CYLINDRICAL_SURFACE('',#8339,0.274999999999999);
#7155=CYLINDRICAL_SURFACE('',#8342,0.274999999999999);
#7156=CYLINDRICAL_SURFACE('',#8367,1.7);
#7157=CYLINDRICAL_SURFACE('',#8370,2.);
#7158=CYLINDRICAL_SURFACE('',#8376,1.1);
#7159=CYLINDRICAL_SURFACE('',#8381,1.5);
#7160=CYLINDRICAL_SURFACE('',#8383,1.7);
#7161=CYLINDRICAL_SURFACE('',#8389,1.5);
#7162=CYLINDRICAL_SURFACE('',#8394,1.2);
#7163=CYLINDRICAL_SURFACE('',#8396,2.);
#7164=CYLINDRICAL_SURFACE('',#8402,1.1);
#7165=CYLINDRICAL_SURFACE('',#8407,1.5);
#7166=CYLINDRICAL_SURFACE('',#8409,1.7);
#7167=CYLINDRICAL_SURFACE('',#8415,1.5);
#7168=CYLINDRICAL_SURFACE('',#8420,1.2);
#7169=CYLINDRICAL_SURFACE('',#8422,2.);
#7170=CYLINDRICAL_SURFACE('',#8428,0.165);
#7171=CYLINDRICAL_SURFACE('',#8432,0.165);
#7172=CYLINDRICAL_SURFACE('',#8436,0.5);
#7173=CYLINDRICAL_SURFACE('',#8442,0.5);
#7174=CYLINDRICAL_SURFACE('',#8447,0.5);
#7175=CYLINDRICAL_SURFACE('',#8452,0.275);
#7176=CYLINDRICAL_SURFACE('',#8454,0.275);
#7177=CYLINDRICAL_SURFACE('',#8456,0.505);
#7178=CYLINDRICAL_SURFACE('',#8466,0.225);
#7179=CYLINDRICAL_SURFACE('',#8469,0.7);
#7180=CYLINDRICAL_SURFACE('',#8475,0.505);
#7181=CYLINDRICAL_SURFACE('',#8478,0.7);
#7182=CYLINDRICAL_SURFACE('',#8491,0.976185);
#7183=CYLINDRICAL_SURFACE('',#8493,0.5);
#7184=CYLINDRICAL_SURFACE('',#8499,0.976185);
#7185=CYLINDRICAL_SURFACE('',#8511,1.023815);
#7186=CYLINDRICAL_SURFACE('',#8518,1.5);
#7187=CYLINDRICAL_SURFACE('',#8523,1.023815);
#7188=CYLINDRICAL_SURFACE('',#8545,1.019052);
#7189=CYLINDRICAL_SURFACE('',#8585,0.980948);
#7190=CYLINDRICAL_SURFACE('',#8599,1.013815);
#7191=CYLINDRICAL_SURFACE('',#8603,0.991185);
#7192=CYLINDRICAL_SURFACE('',#8607,1.013815);
#7193=CYLINDRICAL_SURFACE('',#8611,0.991185);
#7194=CYLINDRICAL_SURFACE('',#8618,0.505);
#7195=CYLINDRICAL_SURFACE('',#8621,0.7);
#7196=CYLINDRICAL_SURFACE('',#8641,0.35);
#7197=CYLINDRICAL_SURFACE('',#8649,0.1954);
#7198=CYLINDRICAL_SURFACE('',#8651,0.225);
#7199=CYLINDRICAL_SURFACE('',#8654,0.7);
#7200=CYLINDRICAL_SURFACE('',#8671,0.2117);
#7201=CYLINDRICAL_SURFACE('',#8695,0.425);
#7202=CYLINDRICAL_SURFACE('',#8703,0.24505);
#7203=CYLINDRICAL_SURFACE('',#8761,0.5);
#7204=CYLINDRICAL_SURFACE('',#8766,0.5);
#7205=CYLINDRICAL_SURFACE('',#8771,0.275);
#7206=CYLINDRICAL_SURFACE('',#8773,0.275);
#7207=CYLINDRICAL_SURFACE('',#8775,0.505);
#7208=ADVANCED_FACE('',(#1007),#7130,.F.);
#7209=ADVANCED_FACE('',(#1008),#7131,.F.);
#7210=ADVANCED_FACE('',(#1009),#7132,.F.);
#7211=ADVANCED_FACE('',(#1010),#7133,.F.);
#7212=ADVANCED_FACE('',(#1011,#609,#610,#611,#612),#702,.T.);
#7213=ADVANCED_FACE('',(#1012),#703,.T.);
#7214=ADVANCED_FACE('',(#1013,#613,#614,#615,#616),#704,.T.);
#7215=ADVANCED_FACE('',(#1014),#705,.T.);
#7216=ADVANCED_FACE('',(#1015),#706,.T.);
#7217=ADVANCED_FACE('',(#1016),#707,.F.);
#7218=ADVANCED_FACE('',(#1017,#617),#7134,.F.);
#7219=ADVANCED_FACE('',(#1018),#7135,.F.);
#7220=ADVANCED_FACE('',(#1019),#708,.F.);
#7221=ADVANCED_FACE('',(#1020),#709,.F.);
#7222=ADVANCED_FACE('',(#1021),#710,.F.);
#7223=ADVANCED_FACE('',(#1022),#711,.F.);
#7224=ADVANCED_FACE('',(#1023),#712,.F.);
#7225=ADVANCED_FACE('',(#1024),#713,.F.);
#7226=ADVANCED_FACE('',(#1025),#714,.F.);
#7227=ADVANCED_FACE('',(#1026),#715,.F.);
#7228=ADVANCED_FACE('',(#1027),#716,.F.);
#7229=ADVANCED_FACE('',(#1028),#717,.F.);
#7230=ADVANCED_FACE('',(#1029),#718,.F.);
#7231=ADVANCED_FACE('',(#1030),#719,.F.);
#7232=ADVANCED_FACE('',(#1031),#720,.F.);
#7233=ADVANCED_FACE('',(#1032,#618),#721,.F.);
#7234=ADVANCED_FACE('',(#1033),#722,.F.);
#7235=ADVANCED_FACE('',(#1034),#723,.F.);
#7236=ADVANCED_FACE('',(#1035),#724,.F.);
#7237=ADVANCED_FACE('',(#1036),#725,.F.);
#7238=ADVANCED_FACE('',(#1037),#726,.F.);
#7239=ADVANCED_FACE('',(#1038),#727,.F.);
#7240=ADVANCED_FACE('',(#1039),#728,.F.);
#7241=ADVANCED_FACE('',(#1040),#729,.F.);
#7242=ADVANCED_FACE('',(#1041),#730,.F.);
#7243=ADVANCED_FACE('',(#1042),#731,.F.);
#7244=ADVANCED_FACE('',(#1043),#732,.F.);
#7245=ADVANCED_FACE('',(#1044),#733,.F.);
#7246=ADVANCED_FACE('',(#1045),#734,.F.);
#7247=ADVANCED_FACE('',(#1046),#735,.F.);
#7248=ADVANCED_FACE('',(#1047),#736,.F.);
#7249=ADVANCED_FACE('',(#1048),#737,.F.);
#7250=ADVANCED_FACE('',(#1049),#738,.F.);
#7251=ADVANCED_FACE('',(#1050,#619),#739,.F.);
#7252=ADVANCED_FACE('',(#1051),#740,.F.);
#7253=ADVANCED_FACE('',(#1052),#741,.F.);
#7254=ADVANCED_FACE('',(#1053),#742,.F.);
#7255=ADVANCED_FACE('',(#1054),#743,.F.);
#7256=ADVANCED_FACE('',(#1055),#7136,.F.);
#7257=ADVANCED_FACE('',(#1056),#744,.T.);
#7258=ADVANCED_FACE('',(#1057),#745,.T.);
#7259=ADVANCED_FACE('',(#1058),#746,.T.);
#7260=ADVANCED_FACE('',(#1059),#747,.T.);
#7261=ADVANCED_FACE('',(#1060),#748,.T.);
#7262=ADVANCED_FACE('',(#1061),#749,.T.);
#7263=ADVANCED_FACE('',(#1062),#750,.T.);
#7264=ADVANCED_FACE('',(#1063),#751,.T.);
#7265=ADVANCED_FACE('',(#1064,#620),#752,.T.);
#7266=ADVANCED_FACE('',(#1065,#621),#753,.F.);
#7267=ADVANCED_FACE('',(#1066,#622),#7137,.F.);
#7268=ADVANCED_FACE('',(#1067),#7138,.F.);
#7269=ADVANCED_FACE('',(#1068),#754,.F.);
#7270=ADVANCED_FACE('',(#1069),#755,.F.);
#7271=ADVANCED_FACE('',(#1070),#756,.F.);
#7272=ADVANCED_FACE('',(#1071),#757,.F.);
#7273=ADVANCED_FACE('',(#1072),#758,.F.);
#7274=ADVANCED_FACE('',(#1073),#759,.F.);
#7275=ADVANCED_FACE('',(#1074),#760,.F.);
#7276=ADVANCED_FACE('',(#1075),#761,.F.);
#7277=ADVANCED_FACE('',(#1076),#762,.F.);
#7278=ADVANCED_FACE('',(#1077),#763,.F.);
#7279=ADVANCED_FACE('',(#1078),#764,.F.);
#7280=ADVANCED_FACE('',(#1079),#765,.F.);
#7281=ADVANCED_FACE('',(#1080),#766,.F.);
#7282=ADVANCED_FACE('',(#1081,#623),#767,.F.);
#7283=ADVANCED_FACE('',(#1082),#768,.F.);
#7284=ADVANCED_FACE('',(#1083),#769,.F.);
#7285=ADVANCED_FACE('',(#1084),#770,.F.);
#7286=ADVANCED_FACE('',(#1085),#771,.F.);
#7287=ADVANCED_FACE('',(#1086),#772,.F.);
#7288=ADVANCED_FACE('',(#1087),#773,.F.);
#7289=ADVANCED_FACE('',(#1088),#774,.F.);
#7290=ADVANCED_FACE('',(#1089),#775,.F.);
#7291=ADVANCED_FACE('',(#1090),#776,.F.);
#7292=ADVANCED_FACE('',(#1091),#777,.F.);
#7293=ADVANCED_FACE('',(#1092),#778,.F.);
#7294=ADVANCED_FACE('',(#1093),#779,.F.);
#7295=ADVANCED_FACE('',(#1094),#780,.F.);
#7296=ADVANCED_FACE('',(#1095),#781,.F.);
#7297=ADVANCED_FACE('',(#1096),#782,.F.);
#7298=ADVANCED_FACE('',(#1097),#783,.F.);
#7299=ADVANCED_FACE('',(#1098),#784,.F.);
#7300=ADVANCED_FACE('',(#1099,#624),#785,.F.);
#7301=ADVANCED_FACE('',(#1100),#786,.F.);
#7302=ADVANCED_FACE('',(#1101),#787,.F.);
#7303=ADVANCED_FACE('',(#1102),#788,.F.);
#7304=ADVANCED_FACE('',(#1103),#789,.F.);
#7305=ADVANCED_FACE('',(#1104),#7139,.F.);
#7306=ADVANCED_FACE('',(#1105),#790,.T.);
#7307=ADVANCED_FACE('',(#1106),#791,.T.);
#7308=ADVANCED_FACE('',(#1107),#792,.T.);
#7309=ADVANCED_FACE('',(#1108),#793,.T.);
#7310=ADVANCED_FACE('',(#1109),#794,.T.);
#7311=ADVANCED_FACE('',(#1110),#795,.T.);
#7312=ADVANCED_FACE('',(#1111),#796,.T.);
#7313=ADVANCED_FACE('',(#1112),#797,.T.);
#7314=ADVANCED_FACE('',(#1113,#625),#798,.T.);
#7315=ADVANCED_FACE('',(#1114,#626),#799,.F.);
#7316=ADVANCED_FACE('',(#1115),#800,.F.);
#7317=ADVANCED_FACE('',(#1116),#801,.F.);
#7318=ADVANCED_FACE('',(#1117),#802,.F.);
#7319=ADVANCED_FACE('',(#1118),#803,.F.);
#7320=ADVANCED_FACE('',(#1119),#804,.F.);
#7321=ADVANCED_FACE('',(#1120),#805,.F.);
#7322=ADVANCED_FACE('',(#1121),#806,.F.);
#7323=ADVANCED_FACE('',(#1122),#807,.F.);
#7324=ADVANCED_FACE('',(#1123),#808,.F.);
#7325=ADVANCED_FACE('',(#1124),#809,.F.);
#7326=ADVANCED_FACE('',(#1125),#810,.F.);
#7327=ADVANCED_FACE('',(#1126),#811,.F.);
#7328=ADVANCED_FACE('',(#1127),#812,.F.);
#7329=ADVANCED_FACE('',(#1128),#813,.F.);
#7330=ADVANCED_FACE('',(#1129),#814,.F.);
#7331=ADVANCED_FACE('',(#1130),#815,.F.);
#7332=ADVANCED_FACE('',(#1131),#816,.F.);
#7333=ADVANCED_FACE('',(#1132),#817,.F.);
#7334=ADVANCED_FACE('',(#1133),#818,.F.);
#7335=ADVANCED_FACE('',(#1134),#819,.F.);
#7336=ADVANCED_FACE('',(#1135),#820,.F.);
#7337=ADVANCED_FACE('',(#1136),#821,.F.);
#7338=ADVANCED_FACE('',(#1137),#822,.F.);
#7339=ADVANCED_FACE('',(#1138),#823,.F.);
#7340=ADVANCED_FACE('',(#1139),#824,.F.);
#7341=ADVANCED_FACE('',(#1140),#825,.F.);
#7342=ADVANCED_FACE('',(#1141),#826,.F.);
#7343=ADVANCED_FACE('',(#1142),#827,.F.);
#7344=ADVANCED_FACE('',(#1143),#828,.F.);
#7345=ADVANCED_FACE('',(#1144),#829,.F.);
#7346=ADVANCED_FACE('',(#1145),#830,.F.);
#7347=ADVANCED_FACE('',(#1146),#831,.F.);
#7348=ADVANCED_FACE('',(#1147),#832,.F.);
#7349=ADVANCED_FACE('',(#1148),#833,.F.);
#7350=ADVANCED_FACE('',(#1149),#834,.F.);
#7351=ADVANCED_FACE('',(#1150),#835,.F.);
#7352=ADVANCED_FACE('',(#1151),#7140,.F.);
#7353=ADVANCED_FACE('',(#1152),#836,.T.);
#7354=ADVANCED_FACE('',(#1153),#837,.T.);
#7355=ADVANCED_FACE('',(#1154),#838,.T.);
#7356=ADVANCED_FACE('',(#1155),#839,.T.);
#7357=ADVANCED_FACE('',(#1156),#840,.T.);
#7358=ADVANCED_FACE('',(#1157),#841,.T.);
#7359=ADVANCED_FACE('',(#1158),#842,.T.);
#7360=ADVANCED_FACE('',(#1159),#843,.T.);
#7361=ADVANCED_FACE('',(#1160,#627),#844,.T.);
#7362=ADVANCED_FACE('',(#1161,#628),#845,.F.);
#7363=ADVANCED_FACE('',(#1162),#846,.F.);
#7364=ADVANCED_FACE('',(#1163),#847,.F.);
#7365=ADVANCED_FACE('',(#1164),#848,.F.);
#7366=ADVANCED_FACE('',(#1165),#849,.F.);
#7367=ADVANCED_FACE('',(#1166),#850,.F.);
#7368=ADVANCED_FACE('',(#1167),#851,.F.);
#7369=ADVANCED_FACE('',(#1168),#852,.F.);
#7370=ADVANCED_FACE('',(#1169),#853,.F.);
#7371=ADVANCED_FACE('',(#1170,#629),#854,.T.);
#7372=ADVANCED_FACE('',(#1171),#7141,.T.);
#7373=ADVANCED_FACE('',(#1172),#855,.F.);
#7374=ADVANCED_FACE('',(#1173),#856,.T.);
#7375=ADVANCED_FACE('',(#1174),#407,.T.);
#7376=ADVANCED_FACE('',(#1175),#7142,.T.);
#7377=ADVANCED_FACE('',(#1176),#408,.T.);
#7378=ADVANCED_FACE('',(#1177,#630),#857,.T.);
#7379=ADVANCED_FACE('',(#1178),#409,.T.);
#7380=ADVANCED_FACE('',(#1179),#7143,.T.);
#7381=ADVANCED_FACE('',(#1180),#858,.T.);
#7382=ADVANCED_FACE('',(#1181),#410,.T.);
#7383=ADVANCED_FACE('',(#1182),#7144,.T.);
#7384=ADVANCED_FACE('',(#1183),#411,.T.);
#7385=ADVANCED_FACE('',(#1184,#631),#859,.T.);
#7386=ADVANCED_FACE('',(#1185),#412,.T.);
#7387=ADVANCED_FACE('',(#1186),#7145,.T.);
#7388=ADVANCED_FACE('',(#1187),#413,.T.);
#7389=ADVANCED_FACE('',(#1188),#860,.T.);
#7390=ADVANCED_FACE('',(#1189),#861,.F.);
#7391=ADVANCED_FACE('',(#1190),#862,.F.);
#7392=ADVANCED_FACE('',(#1191),#863,.F.);
#7393=ADVANCED_FACE('',(#1192),#864,.F.);
#7394=ADVANCED_FACE('',(#1193),#865,.F.);
#7395=ADVANCED_FACE('',(#1194),#866,.F.);
#7396=ADVANCED_FACE('',(#1195),#867,.F.);
#7397=ADVANCED_FACE('',(#1196),#868,.F.);
#7398=ADVANCED_FACE('',(#1197),#7146,.F.);
#7399=ADVANCED_FACE('',(#1198),#7147,.F.);
#7400=ADVANCED_FACE('',(#1199),#7148,.F.);
#7401=ADVANCED_FACE('',(#1200),#7149,.F.);
#7402=ADVANCED_FACE('',(#1201,#632,#633,#634,#635),#869,.T.);
#7403=ADVANCED_FACE('',(#1202),#870,.T.);
#7404=ADVANCED_FACE('',(#1203,#636,#637,#638,#639),#871,.T.);
#7405=ADVANCED_FACE('',(#1204),#872,.T.);
#7406=ADVANCED_FACE('',(#1205),#873,.T.);
#7407=ADVANCED_FACE('',(#1206),#874,.F.);
#7408=ADVANCED_FACE('',(#1207),#414,.F.);
#7409=ADVANCED_FACE('',(#1208),#7150,.F.);
#7410=ADVANCED_FACE('',(#1209,#640),#875,.T.);
#7411=ADVANCED_FACE('',(#1210),#7151,.T.);
#7412=ADVANCED_FACE('',(#1211,#641),#876,.F.);
#7413=ADVANCED_FACE('',(#1212),#7152,.F.);
#7414=ADVANCED_FACE('',(#1213),#7153,.F.);
#7415=ADVANCED_FACE('',(#1214),#877,.T.);
#7416=ADVANCED_FACE('',(#1215),#878,.T.);
#7417=ADVANCED_FACE('',(#1216),#879,.T.);
#7418=ADVANCED_FACE('',(#1217),#880,.T.);
#7419=ADVANCED_FACE('',(#1218,#642,#643),#881,.T.);
#7420=ADVANCED_FACE('',(#1219,#644,#645),#882,.F.);
#7421=ADVANCED_FACE('',(#1220),#883,.T.);
#7422=ADVANCED_FACE('',(#1221),#884,.T.);
#7423=ADVANCED_FACE('',(#1222),#885,.T.);
#7424=ADVANCED_FACE('',(#1223),#886,.T.);
#7425=ADVANCED_FACE('',(#1224),#887,.T.);
#7426=ADVANCED_FACE('',(#1225),#888,.F.);
#7427=ADVANCED_FACE('',(#1226),#889,.T.);
#7428=ADVANCED_FACE('',(#1227),#890,.T.);
#7429=ADVANCED_FACE('',(#1228),#891,.T.);
#7430=ADVANCED_FACE('',(#1229),#892,.T.);
#7431=ADVANCED_FACE('',(#1230),#893,.T.);
#7432=ADVANCED_FACE('',(#1231),#894,.F.);
#7433=ADVANCED_FACE('',(#1232),#7154,.F.);
#7434=ADVANCED_FACE('',(#1233),#7155,.F.);
#7435=ADVANCED_FACE('',(#1234),#895,.T.);
#7436=ADVANCED_FACE('',(#1235),#896,.T.);
#7437=ADVANCED_FACE('',(#1236),#897,.T.);
#7438=ADVANCED_FACE('',(#1237),#898,.T.);
#7439=ADVANCED_FACE('',(#1238,#646,#647),#899,.T.);
#7440=ADVANCED_FACE('',(#1239,#648,#649),#900,.F.);
#7441=ADVANCED_FACE('',(#1240),#901,.T.);
#7442=ADVANCED_FACE('',(#1241),#902,.T.);
#7443=ADVANCED_FACE('',(#1242),#903,.T.);
#7444=ADVANCED_FACE('',(#1243),#904,.T.);
#7445=ADVANCED_FACE('',(#1244),#905,.T.);
#7446=ADVANCED_FACE('',(#1245),#906,.F.);
#7447=ADVANCED_FACE('',(#1246),#907,.T.);
#7448=ADVANCED_FACE('',(#1247),#908,.T.);
#7449=ADVANCED_FACE('',(#1248),#909,.T.);
#7450=ADVANCED_FACE('',(#1249),#910,.T.);
#7451=ADVANCED_FACE('',(#1250),#911,.T.);
#7452=ADVANCED_FACE('',(#1251),#912,.F.);
#7453=ADVANCED_FACE('',(#1252),#7156,.F.);
#7454=ADVANCED_FACE('',(#1253),#7157,.T.);
#7455=ADVANCED_FACE('',(#1254,#650),#913,.T.);
#7456=ADVANCED_FACE('',(#1255,#651),#914,.F.);
#7457=ADVANCED_FACE('',(#1256),#7158,.F.);
#7458=ADVANCED_FACE('',(#1257,#652),#915,.F.);
#7459=ADVANCED_FACE('',(#1258),#7159,.F.);
#7460=ADVANCED_FACE('',(#1259),#7160,.T.);
#7461=ADVANCED_FACE('',(#1260,#653),#916,.T.);
#7462=ADVANCED_FACE('',(#1261,#654),#917,.F.);
#7463=ADVANCED_FACE('',(#1262),#7161,.T.);
#7464=ADVANCED_FACE('',(#1263,#655),#918,.T.);
#7465=ADVANCED_FACE('',(#1264),#7162,.F.);
#7466=ADVANCED_FACE('',(#1265),#7163,.T.);
#7467=ADVANCED_FACE('',(#1266,#656),#919,.T.);
#7468=ADVANCED_FACE('',(#1267,#657),#920,.F.);
#7469=ADVANCED_FACE('',(#1268),#7164,.F.);
#7470=ADVANCED_FACE('',(#1269,#658),#921,.T.);
#7471=ADVANCED_FACE('',(#1270),#7165,.F.);
#7472=ADVANCED_FACE('',(#1271),#7166,.T.);
#7473=ADVANCED_FACE('',(#1272,#659),#922,.T.);
#7474=ADVANCED_FACE('',(#1273,#660),#923,.F.);
#7475=ADVANCED_FACE('',(#1274),#7167,.T.);
#7476=ADVANCED_FACE('',(#1275,#661),#924,.F.);
#7477=ADVANCED_FACE('',(#1276),#7168,.F.);
#7478=ADVANCED_FACE('',(#1277),#7169,.T.);
#7479=ADVANCED_FACE('',(#1278,#662),#925,.T.);
#7480=ADVANCED_FACE('',(#1279,#663),#926,.F.);
#7481=ADVANCED_FACE('',(#1280),#7170,.F.);
#7482=ADVANCED_FACE('',(#1281),#927,.T.);
#7483=ADVANCED_FACE('',(#1282),#7171,.F.);
#7484=ADVANCED_FACE('',(#1283),#928,.F.);
#7485=ADVANCED_FACE('',(#1284),#7172,.T.);
#7486=ADVANCED_FACE('',(#1285,#664),#929,.T.);
#7487=ADVANCED_FACE('',(#1286,#665),#930,.F.);
#7488=ADVANCED_FACE('',(#1287),#7173,.F.);
#7489=ADVANCED_FACE('',(#1288,#666),#931,.T.);
#7490=ADVANCED_FACE('',(#1289),#7174,.F.);
#7491=ADVANCED_FACE('',(#1290,#667),#932,.T.);
#7492=ADVANCED_FACE('',(#1291),#7175,.F.);
#7493=ADVANCED_FACE('',(#1292),#7176,.F.);
#7494=ADVANCED_FACE('',(#1293),#7177,.F.);
#7495=ADVANCED_FACE('',(#1294,#668),#933,.T.);
#7496=ADVANCED_FACE('',(#1295),#934,.T.);
#7497=ADVANCED_FACE('',(#1296,#669),#935,.T.);
#7498=ADVANCED_FACE('',(#1297),#936,.T.);
#7499=ADVANCED_FACE('',(#1298,#670,#671),#937,.T.);
#7500=ADVANCED_FACE('',(#1299,#672,#673),#938,.F.);
#7501=ADVANCED_FACE('',(#1300),#7178,.F.);
#7502=ADVANCED_FACE('',(#1301),#7179,.T.);
#7503=ADVANCED_FACE('',(#1302,#674),#939,.T.);
#7504=ADVANCED_FACE('',(#1303,#675),#940,.F.);
#7505=ADVANCED_FACE('',(#1304),#7180,.F.);
#7506=ADVANCED_FACE('',(#1305),#7181,.T.);
#7507=ADVANCED_FACE('',(#1306,#676),#941,.T.);
#7508=ADVANCED_FACE('',(#1307,#677),#942,.F.);
#7509=ADVANCED_FACE('',(#1308),#405,.F.);
#7510=ADVANCED_FACE('',(#1309),#7182,.T.);
#7511=ADVANCED_FACE('',(#1310),#7183,.F.);
#7512=ADVANCED_FACE('',(#1311),#415,.F.);
#7513=ADVANCED_FACE('',(#1312,#678),#943,.T.);
#7514=ADVANCED_FACE('',(#1313),#7184,.T.);
#7515=ADVANCED_FACE('',(#1314,#679),#944,.T.);
#7516=ADVANCED_FACE('',(#1315),#416,.F.);
#7517=ADVANCED_FACE('',(#1316),#406,.F.);
#7518=ADVANCED_FACE('',(#1317),#7185,.F.);
#7519=ADVANCED_FACE('',(#1318,#680),#945,.T.);
#7520=ADVANCED_FACE('',(#1319),#417,.T.);
#7521=ADVANCED_FACE('',(#1320),#7186,.T.);
#7522=ADVANCED_FACE('',(#1321),#418,.T.);
#7523=ADVANCED_FACE('',(#1322,#681),#946,.T.);
#7524=ADVANCED_FACE('',(#1323),#7187,.F.);
#7525=ADVANCED_FACE('',(#1324),#389,.T.);
#7526=ADVANCED_FACE('',(#1325),#390,.T.);
#7527=ADVANCED_FACE('',(#1326),#391,.T.);
#7528=ADVANCED_FACE('',(#1327),#392,.T.);
#7529=ADVANCED_FACE('',(#1328),#393,.T.);
#7530=ADVANCED_FACE('',(#1329),#394,.T.);
#7531=ADVANCED_FACE('',(#1330),#395,.T.);
#7532=ADVANCED_FACE('',(#1331),#396,.T.);
#7533=ADVANCED_FACE('',(#1332),#397,.F.);
#7534=ADVANCED_FACE('',(#1333),#7188,.T.);
#7535=ADVANCED_FACE('',(#1334),#947,.T.);
#7536=ADVANCED_FACE('',(#1335),#398,.F.);
#7537=ADVANCED_FACE('',(#1336),#948,.T.);
#7538=ADVANCED_FACE('',(#1337),#399,.F.);
#7539=ADVANCED_FACE('',(#1338),#949,.T.);
#7540=ADVANCED_FACE('',(#1339),#400,.F.);
#7541=ADVANCED_FACE('',(#1340),#950,.T.);
#7542=ADVANCED_FACE('',(#1341),#401,.F.);
#7543=ADVANCED_FACE('',(#1342),#951,.T.);
#7544=ADVANCED_FACE('',(#1343),#402,.F.);
#7545=ADVANCED_FACE('',(#1344),#952,.T.);
#7546=ADVANCED_FACE('',(#1345),#403,.F.);
#7547=ADVANCED_FACE('',(#1346),#7189,.F.);
#7548=ADVANCED_FACE('',(#1347),#953,.T.);
#7549=ADVANCED_FACE('',(#1348),#404,.F.);
#7550=ADVANCED_FACE('',(#1349,#682),#954,.T.);
#7551=ADVANCED_FACE('',(#1350),#955,.T.);
#7552=ADVANCED_FACE('',(#1351,#683),#956,.T.);
#7553=ADVANCED_FACE('',(#1352),#7190,.T.);
#7554=ADVANCED_FACE('',(#1353,#684),#957,.T.);
#7555=ADVANCED_FACE('',(#1354),#7191,.F.);
#7556=ADVANCED_FACE('',(#1355,#685),#958,.T.);
#7557=ADVANCED_FACE('',(#1356),#7192,.T.);
#7558=ADVANCED_FACE('',(#1357,#686),#959,.T.);
#7559=ADVANCED_FACE('',(#1358),#7193,.F.);
#7560=ADVANCED_FACE('',(#1359),#7194,.F.);
#7561=ADVANCED_FACE('',(#1360),#7195,.T.);
#7562=ADVANCED_FACE('',(#1361,#687),#960,.T.);
#7563=ADVANCED_FACE('',(#1362,#688),#961,.F.);
#7564=ADVANCED_FACE('',(#1363),#962,.F.);
#7565=ADVANCED_FACE('',(#1364),#963,.F.);
#7566=ADVANCED_FACE('',(#1365),#964,.F.);
#7567=ADVANCED_FACE('',(#1366),#965,.F.);
#7568=ADVANCED_FACE('',(#1367),#966,.F.);
#7569=ADVANCED_FACE('',(#1368),#967,.F.);
#7570=ADVANCED_FACE('',(#1369),#968,.F.);
#7571=ADVANCED_FACE('',(#1370),#969,.F.);
#7572=ADVANCED_FACE('',(#1371),#970,.F.);
#7573=ADVANCED_FACE('',(#1372),#971,.T.);
#7574=ADVANCED_FACE('',(#1373),#419,.T.);
#7575=ADVANCED_FACE('',(#1374),#7196,.T.);
#7576=ADVANCED_FACE('',(#1375),#420,.T.);
#7577=ADVANCED_FACE('',(#1376,#689),#972,.T.);
#7578=ADVANCED_FACE('',(#1377),#421,.T.);
#7579=ADVANCED_FACE('',(#1378),#7197,.T.);
#7580=ADVANCED_FACE('',(#1379),#7198,.F.);
#7581=ADVANCED_FACE('',(#1380),#7199,.T.);
#7582=ADVANCED_FACE('',(#1381,#690),#973,.T.);
#7583=ADVANCED_FACE('',(#1382,#691),#974,.F.);
#7584=ADVANCED_FACE('',(#1383),#975,.F.);
#7585=ADVANCED_FACE('',(#1384),#976,.T.);
#7586=ADVANCED_FACE('',(#1385,#692),#977,.T.);
#7587=ADVANCED_FACE('',(#1386),#978,.T.);
#7588=ADVANCED_FACE('',(#1387),#979,.T.);
#7589=ADVANCED_FACE('',(#1388),#980,.F.);
#7590=ADVANCED_FACE('',(#1389),#981,.T.);
#7591=ADVANCED_FACE('',(#1390),#982,.T.);
#7592=ADVANCED_FACE('',(#1391),#983,.T.);
#7593=ADVANCED_FACE('',(#1392),#7200,.F.);
#7594=ADVANCED_FACE('',(#1393),#984,.F.);
#7595=ADVANCED_FACE('',(#1394),#985,.F.);
#7596=ADVANCED_FACE('',(#1395),#986,.T.);
#7597=ADVANCED_FACE('',(#1396),#987,.T.);
#7598=ADVANCED_FACE('',(#1397),#988,.F.);
#7599=ADVANCED_FACE('',(#1398),#989,.F.);
#7600=ADVANCED_FACE('',(#1399),#990,.F.);
#7601=ADVANCED_FACE('',(#1400),#991,.F.);
#7602=ADVANCED_FACE('',(#1401),#992,.F.);
#7603=ADVANCED_FACE('',(#1402),#993,.F.);
#7604=ADVANCED_FACE('',(#1403),#994,.F.);
#7605=ADVANCED_FACE('',(#1404),#995,.F.);
#7606=ADVANCED_FACE('',(#1405),#996,.F.);
#7607=ADVANCED_FACE('',(#1406),#997,.T.);
#7608=ADVANCED_FACE('',(#1407),#422,.T.);
#7609=ADVANCED_FACE('',(#1408),#7201,.T.);
#7610=ADVANCED_FACE('',(#1409),#423,.T.);
#7611=ADVANCED_FACE('',(#1410,#693),#998,.T.);
#7612=ADVANCED_FACE('',(#1411),#424,.T.);
#7613=ADVANCED_FACE('',(#1412),#7202,.T.);
#7614=ADVANCED_FACE('',(#1413),#7203,.F.);
#7615=ADVANCED_FACE('',(#1414,#694),#999,.T.);
#7616=ADVANCED_FACE('',(#1415),#7204,.F.);
#7617=ADVANCED_FACE('',(#1416,#695),#1000,.T.);
#7618=ADVANCED_FACE('',(#1417),#7205,.F.);
#7619=ADVANCED_FACE('',(#1418),#7206,.F.);
#7620=ADVANCED_FACE('',(#1419),#7207,.F.);
#7621=ADVANCED_FACE('',(#1420,#696),#1001,.T.);
#7622=ADVANCED_FACE('',(#1421),#1002,.T.);
#7623=ADVANCED_FACE('',(#1422,#697),#1003,.T.);
#7624=ADVANCED_FACE('',(#1423),#1004,.T.);
#7625=ADVANCED_FACE('',(#1424,#698,#699),#1005,.T.);
#7626=ADVANCED_FACE('',(#1425,#700,#701),#1006,.F.);
#7627=CLOSED_SHELL('',(#7208,#7209,#7210,#7211,#7212,#7213,#7214,#7215,
#7216,#7217));
#7628=CLOSED_SHELL('',(#7218,#7219,#7220,#7221,#7222,#7223,#7224,#7225,
#7226,#7227,#7228,#7229,#7230,#7231,#7232,#7233,#7234,#7235,#7236,#7237,
#7238,#7239,#7240,#7241,#7242,#7243,#7244,#7245,#7246,#7247,#7248,#7249,
#7250,#7251,#7252,#7253,#7254,#7255,#7256,#7257,#7258,#7259,#7260,#7261,
#7262,#7263,#7264,#7265,#7266));
#7629=CLOSED_SHELL('',(#7267,#7268,#7269,#7270,#7271,#7272,#7273,#7274,
#7275,#7276,#7277,#7278,#7279,#7280,#7281,#7282,#7283,#7284,#7285,#7286,
#7287,#7288,#7289,#7290,#7291,#7292,#7293,#7294,#7295,#7296,#7297,#7298,
#7299,#7300,#7301,#7302,#7303,#7304,#7305,#7306,#7307,#7308,#7309,#7310,
#7311,#7312,#7313,#7314,#7315));
#7630=CLOSED_SHELL('',(#7316,#7317,#7318,#7319,#7320,#7321,#7322,#7323,
#7324,#7325,#7326,#7327,#7328,#7329,#7330,#7331,#7332,#7333,#7334,#7335,
#7336,#7337,#7338,#7339,#7340,#7341,#7342,#7343,#7344,#7345,#7346,#7347,
#7348,#7349,#7350,#7351,#7352,#7353,#7354,#7355,#7356,#7357,#7358,#7359,
#7360,#7361,#7362));
#7631=CLOSED_SHELL('',(#7363,#7364,#7365,#7366,#7367,#7368,#7369,#7370));
#7632=CLOSED_SHELL('',(#7371,#7372,#7373,#7374,#7375,#7376,#7377,#7378,
#7379,#7380));
#7633=CLOSED_SHELL('',(#7381,#7382,#7383,#7384,#7385,#7386,#7387,#7388,
#7389));
#7634=CLOSED_SHELL('',(#7390,#7391,#7392,#7393,#7394,#7395,#7396,#7397));
#7635=CLOSED_SHELL('',(#7398,#7399,#7400,#7401,#7402,#7403,#7404,#7405,
#7406,#7407));
#7636=CLOSED_SHELL('',(#7408,#7409,#7410,#7411,#7412));
#7637=CLOSED_SHELL('',(#7413,#7414,#7415,#7416,#7417,#7418,#7419,#7420));
#7638=CLOSED_SHELL('',(#7421,#7422,#7423,#7424,#7425,#7426));
#7639=CLOSED_SHELL('',(#7427,#7428,#7429,#7430,#7431,#7432));
#7640=CLOSED_SHELL('',(#7433,#7434,#7435,#7436,#7437,#7438,#7439,#7440));
#7641=CLOSED_SHELL('',(#7441,#7442,#7443,#7444,#7445,#7446));
#7642=CLOSED_SHELL('',(#7447,#7448,#7449,#7450,#7451,#7452));
#7643=CLOSED_SHELL('',(#7453,#7454,#7455,#7456));
#7644=CLOSED_SHELL('',(#7457,#7458,#7459,#7460,#7461,#7462));
#7645=CLOSED_SHELL('',(#7463,#7464,#7465,#7466,#7467,#7468));
#7646=CLOSED_SHELL('',(#7469,#7470,#7471,#7472,#7473,#7474));
#7647=CLOSED_SHELL('',(#7475,#7476,#7477,#7478,#7479,#7480));
#7648=CLOSED_SHELL('',(#7481,#7482,#7483,#7484,#7485,#7486,#7487));
#7649=CLOSED_SHELL('',(#7488,#7489,#7490,#7491,#7492,#7493,#7494,#7495,
#7496,#7497,#7498,#7499,#7500));
#7650=CLOSED_SHELL('',(#7501,#7502,#7503,#7504));
#7651=CLOSED_SHELL('',(#7505,#7506,#7507,#7508));
#7652=CLOSED_SHELL('',(#7509,#7510,#7511,#7512,#7513,#7514,#7515,#7516));
#7653=CLOSED_SHELL('',(#7517,#7518,#7519,#7520,#7521,#7522,#7523,#7524));
#7654=CLOSED_SHELL('',(#7525));
#7655=CLOSED_SHELL('',(#7526));
#7656=CLOSED_SHELL('',(#7527));
#7657=CLOSED_SHELL('',(#7528));
#7658=CLOSED_SHELL('',(#7529));
#7659=CLOSED_SHELL('',(#7530));
#7660=CLOSED_SHELL('',(#7531));
#7661=CLOSED_SHELL('',(#7532));
#7662=CLOSED_SHELL('',(#7533,#7534,#7535,#7536,#7537,#7538,#7539,#7540,
#7541,#7542,#7543,#7544,#7545,#7546,#7547,#7548,#7549,#7550,#7551));
#7663=CLOSED_SHELL('',(#7552,#7553,#7554,#7555));
#7664=CLOSED_SHELL('',(#7556,#7557,#7558,#7559));
#7665=CLOSED_SHELL('',(#7560,#7561,#7562,#7563));
#7666=CLOSED_SHELL('',(#7564,#7565,#7566,#7567,#7568,#7569,#7570,#7571));
#7667=CLOSED_SHELL('',(#7572,#7573,#7574,#7575,#7576,#7577,#7578,#7579));
#7668=CLOSED_SHELL('',(#7580,#7581,#7582,#7583));
#7669=CLOSED_SHELL('',(#7584,#7585,#7586,#7587,#7588,#7589,#7590,#7591,
#7592,#7593,#7594,#7595,#7596,#7597));
#7670=CLOSED_SHELL('',(#7598,#7599,#7600,#7601,#7602,#7603,#7604,#7605));
#7671=CLOSED_SHELL('',(#7606,#7607,#7608,#7609,#7610,#7611,#7612,#7613));
#7672=CLOSED_SHELL('',(#7614,#7615,#7616,#7617,#7618,#7619,#7620,#7621,
#7622,#7623,#7624,#7625,#7626));
#7673=DERIVED_UNIT_ELEMENT(#7741,1.);
#7674=DERIVED_UNIT_ELEMENT(#13823,-3.);
#7675=DERIVED_UNIT_ELEMENT(#7741,1.);
#7676=DERIVED_UNIT_ELEMENT(#13823,-3.);
#7677=DERIVED_UNIT_ELEMENT(#7741,1.);
#7678=DERIVED_UNIT_ELEMENT(#13823,-3.);
#7679=DERIVED_UNIT_ELEMENT(#7741,1.);
#7680=DERIVED_UNIT_ELEMENT(#13823,-3.);
#7681=DERIVED_UNIT_ELEMENT(#7741,1.);
#7682=DERIVED_UNIT_ELEMENT(#13823,-3.);
#7683=DERIVED_UNIT_ELEMENT(#7741,1.);
#7684=DERIVED_UNIT_ELEMENT(#13823,-3.);
#7685=DERIVED_UNIT_ELEMENT(#7741,1.);
#7686=DERIVED_UNIT_ELEMENT(#13823,-3.);
#7687=DERIVED_UNIT_ELEMENT(#7741,1.);
#7688=DERIVED_UNIT_ELEMENT(#13823,-3.);
#7689=DERIVED_UNIT_ELEMENT(#7741,1.);
#7690=DERIVED_UNIT_ELEMENT(#13823,-3.);
#7691=DERIVED_UNIT_ELEMENT(#7741,1.);
#7692=DERIVED_UNIT_ELEMENT(#13823,-3.);
#7693=DERIVED_UNIT_ELEMENT(#7741,1.);
#7694=DERIVED_UNIT_ELEMENT(#13823,-3.);
#7695=DERIVED_UNIT_ELEMENT(#7741,1.);
#7696=DERIVED_UNIT_ELEMENT(#13823,-3.);
#7697=DERIVED_UNIT_ELEMENT(#7741,1.);
#7698=DERIVED_UNIT_ELEMENT(#13823,-3.);
#7699=DERIVED_UNIT_ELEMENT(#7741,1.);
#7700=DERIVED_UNIT_ELEMENT(#13823,-3.);
#7701=DERIVED_UNIT_ELEMENT(#7741,1.);
#7702=DERIVED_UNIT_ELEMENT(#13823,-3.);
#7703=DERIVED_UNIT_ELEMENT(#7741,1.);
#7704=DERIVED_UNIT_ELEMENT(#13823,-3.);
#7705=DERIVED_UNIT_ELEMENT(#7741,1.);
#7706=DERIVED_UNIT_ELEMENT(#13823,-3.);
#7707=DERIVED_UNIT_ELEMENT(#7741,1.);
#7708=DERIVED_UNIT_ELEMENT(#13823,-3.);
#7709=DERIVED_UNIT_ELEMENT(#7741,1.);
#7710=DERIVED_UNIT_ELEMENT(#13823,-3.);
#7711=DERIVED_UNIT_ELEMENT(#7741,1.);
#7712=DERIVED_UNIT_ELEMENT(#13823,-3.);
#7713=DERIVED_UNIT_ELEMENT(#7741,1.);
#7714=DERIVED_UNIT_ELEMENT(#13823,-3.);
#7715=DERIVED_UNIT_ELEMENT(#7741,1.);
#7716=DERIVED_UNIT_ELEMENT(#13823,-3.);
#7717=DERIVED_UNIT_ELEMENT(#7741,1.);
#7718=DERIVED_UNIT_ELEMENT(#13823,-3.);
#7719=DERIVED_UNIT_ELEMENT(#7741,1.);
#7720=DERIVED_UNIT_ELEMENT(#13823,-3.);
#7721=DERIVED_UNIT_ELEMENT(#7741,1.);
#7722=DERIVED_UNIT_ELEMENT(#13823,-3.);
#7723=DERIVED_UNIT_ELEMENT(#7741,1.);
#7724=DERIVED_UNIT_ELEMENT(#13823,-3.);
#7725=DERIVED_UNIT_ELEMENT(#7741,1.);
#7726=DERIVED_UNIT_ELEMENT(#13823,-3.);
#7727=DERIVED_UNIT_ELEMENT(#7741,1.);
#7728=DERIVED_UNIT_ELEMENT(#13823,-3.);
#7729=DERIVED_UNIT_ELEMENT(#7741,1.);
#7730=DERIVED_UNIT_ELEMENT(#13823,-3.);
#7731=DERIVED_UNIT_ELEMENT(#7741,1.);
#7732=DERIVED_UNIT_ELEMENT(#13823,-3.);
#7733=DERIVED_UNIT_ELEMENT(#7741,1.);
#7734=DERIVED_UNIT_ELEMENT(#13823,-3.);
#7735=DERIVED_UNIT_ELEMENT(#7741,1.);
#7736=DERIVED_UNIT_ELEMENT(#13823,-3.);
#7737=DERIVED_UNIT_ELEMENT(#7741,1.);
#7738=DERIVED_UNIT_ELEMENT(#13823,-3.);
#7739=DERIVED_UNIT_ELEMENT(#7741,1.);
#7740=DERIVED_UNIT_ELEMENT(#13823,-3.);
#7741=(
MASS_UNIT()
NAMED_UNIT(*)
SI_UNIT(.KILO.,.GRAM.)
);
#7742=DERIVED_UNIT((#7673,#7674));
#7743=DERIVED_UNIT((#7675,#7676));
#7744=DERIVED_UNIT((#7677,#7678));
#7745=DERIVED_UNIT((#7679,#7680));
#7746=DERIVED_UNIT((#7681,#7682));
#7747=DERIVED_UNIT((#7683,#7684));
#7748=DERIVED_UNIT((#7685,#7686));
#7749=DERIVED_UNIT((#7687,#7688));
#7750=DERIVED_UNIT((#7689,#7690));
#7751=DERIVED_UNIT((#7691,#7692));
#7752=DERIVED_UNIT((#7693,#7694));
#7753=DERIVED_UNIT((#7695,#7696));
#7754=DERIVED_UNIT((#7697,#7698));
#7755=DERIVED_UNIT((#7699,#7700));
#7756=DERIVED_UNIT((#7701,#7702));
#7757=DERIVED_UNIT((#7703,#7704));
#7758=DERIVED_UNIT((#7705,#7706));
#7759=DERIVED_UNIT((#7707,#7708));
#7760=DERIVED_UNIT((#7709,#7710));
#7761=DERIVED_UNIT((#7711,#7712));
#7762=DERIVED_UNIT((#7713,#7714));
#7763=DERIVED_UNIT((#7715,#7716));
#7764=DERIVED_UNIT((#7717,#7718));
#7765=DERIVED_UNIT((#7719,#7720));
#7766=DERIVED_UNIT((#7721,#7722));
#7767=DERIVED_UNIT((#7723,#7724));
#7768=DERIVED_UNIT((#7725,#7726));
#7769=DERIVED_UNIT((#7727,#7728));
#7770=DERIVED_UNIT((#7729,#7730));
#7771=DERIVED_UNIT((#7731,#7732));
#7772=DERIVED_UNIT((#7733,#7734));
#7773=DERIVED_UNIT((#7735,#7736));
#7774=DERIVED_UNIT((#7737,#7738));
#7775=DERIVED_UNIT((#7739,#7740));
#7776=MEASURE_REPRESENTATION_ITEM('density measure',
POSITIVE_RATIO_MEASURE(7850.),#7742);
#7777=MEASURE_REPRESENTATION_ITEM('density measure',
POSITIVE_RATIO_MEASURE(7850.),#7743);
#7778=MEASURE_REPRESENTATION_ITEM('density measure',
POSITIVE_RATIO_MEASURE(7850.),#7744);
#7779=MEASURE_REPRESENTATION_ITEM('density measure',
POSITIVE_RATIO_MEASURE(7850.),#7745);
#7780=MEASURE_REPRESENTATION_ITEM('density measure',
POSITIVE_RATIO_MEASURE(7850.),#7746);
#7781=MEASURE_REPRESENTATION_ITEM('density measure',
POSITIVE_RATIO_MEASURE(7850.),#7747);
#7782=MEASURE_REPRESENTATION_ITEM('density measure',
POSITIVE_RATIO_MEASURE(7850.),#7748);
#7783=MEASURE_REPRESENTATION_ITEM('density measure',
POSITIVE_RATIO_MEASURE(7850.),#7749);
#7784=MEASURE_REPRESENTATION_ITEM('density measure',
POSITIVE_RATIO_MEASURE(7850.),#7750);
#7785=MEASURE_REPRESENTATION_ITEM('density measure',
POSITIVE_RATIO_MEASURE(7850.),#7751);
#7786=MEASURE_REPRESENTATION_ITEM('density measure',
POSITIVE_RATIO_MEASURE(7850.),#7752);
#7787=MEASURE_REPRESENTATION_ITEM('density measure',
POSITIVE_RATIO_MEASURE(7850.),#7753);
#7788=MEASURE_REPRESENTATION_ITEM('density measure',
POSITIVE_RATIO_MEASURE(7850.),#7754);
#7789=MEASURE_REPRESENTATION_ITEM('density measure',
POSITIVE_RATIO_MEASURE(7850.),#7755);
#7790=MEASURE_REPRESENTATION_ITEM('density measure',
POSITIVE_RATIO_MEASURE(7850.),#7756);
#7791=MEASURE_REPRESENTATION_ITEM('density measure',
POSITIVE_RATIO_MEASURE(7850.),#7757);
#7792=MEASURE_REPRESENTATION_ITEM('density measure',
POSITIVE_RATIO_MEASURE(7850.),#7758);
#7793=MEASURE_REPRESENTATION_ITEM('density measure',
POSITIVE_RATIO_MEASURE(7850.),#7759);
#7794=MEASURE_REPRESENTATION_ITEM('density measure',
POSITIVE_RATIO_MEASURE(7850.),#7760);
#7795=MEASURE_REPRESENTATION_ITEM('density measure',
POSITIVE_RATIO_MEASURE(7850.),#7761);
#7796=MEASURE_REPRESENTATION_ITEM('density measure',
POSITIVE_RATIO_MEASURE(7850.),#7762);
#7797=MEASURE_REPRESENTATION_ITEM('density measure',
POSITIVE_RATIO_MEASURE(7850.),#7763);
#7798=MEASURE_REPRESENTATION_ITEM('density measure',
POSITIVE_RATIO_MEASURE(7850.),#7764);
#7799=MEASURE_REPRESENTATION_ITEM('density measure',
POSITIVE_RATIO_MEASURE(7850.),#7765);
#7800=MEASURE_REPRESENTATION_ITEM('density measure',
POSITIVE_RATIO_MEASURE(7850.),#7766);
#7801=MEASURE_REPRESENTATION_ITEM('density measure',
POSITIVE_RATIO_MEASURE(7850.),#7767);
#7802=MEASURE_REPRESENTATION_ITEM('density measure',
POSITIVE_RATIO_MEASURE(7850.),#7768);
#7803=MEASURE_REPRESENTATION_ITEM('density measure',
POSITIVE_RATIO_MEASURE(7850.),#7769);
#7804=MEASURE_REPRESENTATION_ITEM('density measure',
POSITIVE_RATIO_MEASURE(7850.),#7770);
#7805=MEASURE_REPRESENTATION_ITEM('density measure',
POSITIVE_RATIO_MEASURE(7850.),#7771);
#7806=MEASURE_REPRESENTATION_ITEM('density measure',
POSITIVE_RATIO_MEASURE(7850.),#7772);
#7807=MEASURE_REPRESENTATION_ITEM('density measure',
POSITIVE_RATIO_MEASURE(7850.),#7773);
#7808=MEASURE_REPRESENTATION_ITEM('density measure',
POSITIVE_RATIO_MEASURE(7850.),#7774);
#7809=MEASURE_REPRESENTATION_ITEM('density measure',
POSITIVE_RATIO_MEASURE(7850.),#7775);
#7810=PROPERTY_DEFINITION_REPRESENTATION(#7980,#7878);
#7811=PROPERTY_DEFINITION_REPRESENTATION(#7981,#7879);
#7812=PROPERTY_DEFINITION_REPRESENTATION(#7982,#7880);
#7813=PROPERTY_DEFINITION_REPRESENTATION(#7983,#7881);
#7814=PROPERTY_DEFINITION_REPRESENTATION(#7984,#7882);
#7815=PROPERTY_DEFINITION_REPRESENTATION(#7985,#7883);
#7816=PROPERTY_DEFINITION_REPRESENTATION(#7986,#7884);
#7817=PROPERTY_DEFINITION_REPRESENTATION(#7987,#7885);
#7818=PROPERTY_DEFINITION_REPRESENTATION(#7988,#7886);
#7819=PROPERTY_DEFINITION_REPRESENTATION(#7989,#7887);
#7820=PROPERTY_DEFINITION_REPRESENTATION(#7990,#7888);
#7821=PROPERTY_DEFINITION_REPRESENTATION(#7991,#7889);
#7822=PROPERTY_DEFINITION_REPRESENTATION(#7992,#7890);
#7823=PROPERTY_DEFINITION_REPRESENTATION(#7993,#7891);
#7824=PROPERTY_DEFINITION_REPRESENTATION(#7994,#7892);
#7825=PROPERTY_DEFINITION_REPRESENTATION(#7995,#7893);
#7826=PROPERTY_DEFINITION_REPRESENTATION(#7996,#7894);
#7827=PROPERTY_DEFINITION_REPRESENTATION(#7997,#7895);
#7828=PROPERTY_DEFINITION_REPRESENTATION(#7998,#7896);
#7829=PROPERTY_DEFINITION_REPRESENTATION(#7999,#7897);
#7830=PROPERTY_DEFINITION_REPRESENTATION(#8000,#7898);
#7831=PROPERTY_DEFINITION_REPRESENTATION(#8001,#7899);
#7832=PROPERTY_DEFINITION_REPRESENTATION(#8002,#7900);
#7833=PROPERTY_DEFINITION_REPRESENTATION(#8003,#7901);
#7834=PROPERTY_DEFINITION_REPRESENTATION(#8004,#7902);
#7835=PROPERTY_DEFINITION_REPRESENTATION(#8005,#7903);
#7836=PROPERTY_DEFINITION_REPRESENTATION(#8006,#7904);
#7837=PROPERTY_DEFINITION_REPRESENTATION(#8007,#7905);
#7838=PROPERTY_DEFINITION_REPRESENTATION(#8008,#7906);
#7839=PROPERTY_DEFINITION_REPRESENTATION(#8009,#7907);
#7840=PROPERTY_DEFINITION_REPRESENTATION(#8010,#7908);
#7841=PROPERTY_DEFINITION_REPRESENTATION(#8011,#7909);
#7842=PROPERTY_DEFINITION_REPRESENTATION(#8012,#7910);
#7843=PROPERTY_DEFINITION_REPRESENTATION(#8013,#7911);
#7844=PROPERTY_DEFINITION_REPRESENTATION(#8014,#7912);
#7845=PROPERTY_DEFINITION_REPRESENTATION(#8015,#7913);
#7846=PROPERTY_DEFINITION_REPRESENTATION(#8016,#7914);
#7847=PROPERTY_DEFINITION_REPRESENTATION(#8017,#7915);
#7848=PROPERTY_DEFINITION_REPRESENTATION(#8018,#7916);
#7849=PROPERTY_DEFINITION_REPRESENTATION(#8019,#7917);
#7850=PROPERTY_DEFINITION_REPRESENTATION(#8020,#7918);
#7851=PROPERTY_DEFINITION_REPRESENTATION(#8021,#7919);
#7852=PROPERTY_DEFINITION_REPRESENTATION(#8022,#7920);
#7853=PROPERTY_DEFINITION_REPRESENTATION(#8023,#7921);
#7854=PROPERTY_DEFINITION_REPRESENTATION(#8024,#7922);
#7855=PROPERTY_DEFINITION_REPRESENTATION(#8025,#7923);
#7856=PROPERTY_DEFINITION_REPRESENTATION(#8026,#7924);
#7857=PROPERTY_DEFINITION_REPRESENTATION(#8027,#7925);
#7858=PROPERTY_DEFINITION_REPRESENTATION(#8028,#7926);
#7859=PROPERTY_DEFINITION_REPRESENTATION(#8029,#7927);
#7860=PROPERTY_DEFINITION_REPRESENTATION(#8030,#7928);
#7861=PROPERTY_DEFINITION_REPRESENTATION(#8031,#7929);
#7862=PROPERTY_DEFINITION_REPRESENTATION(#8032,#7930);
#7863=PROPERTY_DEFINITION_REPRESENTATION(#8033,#7931);
#7864=PROPERTY_DEFINITION_REPRESENTATION(#8034,#7932);
#7865=PROPERTY_DEFINITION_REPRESENTATION(#8035,#7933);
#7866=PROPERTY_DEFINITION_REPRESENTATION(#8036,#7934);
#7867=PROPERTY_DEFINITION_REPRESENTATION(#8037,#7935);
#7868=PROPERTY_DEFINITION_REPRESENTATION(#8038,#7936);
#7869=PROPERTY_DEFINITION_REPRESENTATION(#8039,#7937);
#7870=PROPERTY_DEFINITION_REPRESENTATION(#8040,#7938);
#7871=PROPERTY_DEFINITION_REPRESENTATION(#8041,#7939);
#7872=PROPERTY_DEFINITION_REPRESENTATION(#8042,#7940);
#7873=PROPERTY_DEFINITION_REPRESENTATION(#8043,#7941);
#7874=PROPERTY_DEFINITION_REPRESENTATION(#8044,#7942);
#7875=PROPERTY_DEFINITION_REPRESENTATION(#8045,#7943);
#7876=PROPERTY_DEFINITION_REPRESENTATION(#8046,#7944);
#7877=PROPERTY_DEFINITION_REPRESENTATION(#8047,#7945);
#7878=REPRESENTATION('material name',(#7946),#13785);
#7879=REPRESENTATION('density',(#7776),#13785);
#7880=REPRESENTATION('material name',(#7947),#13786);
#7881=REPRESENTATION('density',(#7777),#13786);
#7882=REPRESENTATION('material name',(#7948),#13787);
#7883=REPRESENTATION('density',(#7778),#13787);
#7884=REPRESENTATION('material name',(#7949),#13788);
#7885=REPRESENTATION('density',(#7779),#13788);
#7886=REPRESENTATION('material name',(#7950),#13789);
#7887=REPRESENTATION('density',(#7780),#13789);
#7888=REPRESENTATION('material name',(#7951),#13790);
#7889=REPRESENTATION('density',(#7781),#13790);
#7890=REPRESENTATION('material name',(#7952),#13791);
#7891=REPRESENTATION('density',(#7782),#13791);
#7892=REPRESENTATION('material name',(#7953),#13792);
#7893=REPRESENTATION('density',(#7783),#13792);
#7894=REPRESENTATION('material name',(#7954),#13793);
#7895=REPRESENTATION('density',(#7784),#13793);
#7896=REPRESENTATION('material name',(#7955),#13794);
#7897=REPRESENTATION('density',(#7785),#13794);
#7898=REPRESENTATION('material name',(#7956),#13795);
#7899=REPRESENTATION('density',(#7786),#13795);
#7900=REPRESENTATION('material name',(#7957),#13796);
#7901=REPRESENTATION('density',(#7787),#13796);
#7902=REPRESENTATION('material name',(#7958),#13797);
#7903=REPRESENTATION('density',(#7788),#13797);
#7904=REPRESENTATION('material name',(#7959),#13798);
#7905=REPRESENTATION('density',(#7789),#13798);
#7906=REPRESENTATION('material name',(#7960),#13800);
#7907=REPRESENTATION('density',(#7790),#13800);
#7908=REPRESENTATION('material name',(#7961),#13801);
#7909=REPRESENTATION('density',(#7791),#13801);
#7910=REPRESENTATION('material name',(#7962),#13802);
#7911=REPRESENTATION('density',(#7792),#13802);
#7912=REPRESENTATION('material name',(#7963),#13803);
#7913=REPRESENTATION('density',(#7793),#13803);
#7914=REPRESENTATION('material name',(#7964),#13804);
#7915=REPRESENTATION('density',(#7794),#13804);
#7916=REPRESENTATION('material name',(#7965),#13805);
#7917=REPRESENTATION('density',(#7795),#13805);
#7918=REPRESENTATION('material name',(#7966),#13806);
#7919=REPRESENTATION('density',(#7796),#13806);
#7920=REPRESENTATION('material name',(#7967),#13807);
#7921=REPRESENTATION('density',(#7797),#13807);
#7922=REPRESENTATION('material name',(#7968),#13808);
#7923=REPRESENTATION('density',(#7798),#13808);
#7924=REPRESENTATION('material name',(#7969),#13810);
#7925=REPRESENTATION('density',(#7799),#13810);
#7926=REPRESENTATION('material name',(#7970),#13811);
#7927=REPRESENTATION('density',(#7800),#13811);
#7928=REPRESENTATION('material name',(#7971),#13812);
#7929=REPRESENTATION('density',(#7801),#13812);
#7930=REPRESENTATION('material name',(#7972),#13813);
#7931=REPRESENTATION('density',(#7802),#13813);
#7932=REPRESENTATION('material name',(#7973),#13814);
#7933=REPRESENTATION('density',(#7803),#13814);
#7934=REPRESENTATION('material name',(#7974),#13815);
#7935=REPRESENTATION('density',(#7804),#13815);
#7936=REPRESENTATION('material name',(#7975),#13816);
#7937=REPRESENTATION('density',(#7805),#13816);
#7938=REPRESENTATION('material name',(#7976),#13817);
#7939=REPRESENTATION('density',(#7806),#13817);
#7940=REPRESENTATION('material name',(#7977),#13818);
#7941=REPRESENTATION('density',(#7807),#13818);
#7942=REPRESENTATION('material name',(#7978),#13819);
#7943=REPRESENTATION('density',(#7808),#13819);
#7944=REPRESENTATION('material name',(#7979),#13820);
#7945=REPRESENTATION('density',(#7809),#13820);
#7946=DESCRIPTIVE_REPRESENTATION_ITEM('Steel','Steel');
#7947=DESCRIPTIVE_REPRESENTATION_ITEM('Steel','Steel');
#7948=DESCRIPTIVE_REPRESENTATION_ITEM('Steel','Steel');
#7949=DESCRIPTIVE_REPRESENTATION_ITEM('Steel','Steel');
#7950=DESCRIPTIVE_REPRESENTATION_ITEM('Steel','Steel');
#7951=DESCRIPTIVE_REPRESENTATION_ITEM('Steel','Steel');
#7952=DESCRIPTIVE_REPRESENTATION_ITEM('Steel','Steel');
#7953=DESCRIPTIVE_REPRESENTATION_ITEM('Steel','Steel');
#7954=DESCRIPTIVE_REPRESENTATION_ITEM('Steel','Steel');
#7955=DESCRIPTIVE_REPRESENTATION_ITEM('Steel','Steel');
#7956=DESCRIPTIVE_REPRESENTATION_ITEM('Steel','Steel');
#7957=DESCRIPTIVE_REPRESENTATION_ITEM('Steel','Steel');
#7958=DESCRIPTIVE_REPRESENTATION_ITEM('Steel','Steel');
#7959=DESCRIPTIVE_REPRESENTATION_ITEM('Steel','Steel');
#7960=DESCRIPTIVE_REPRESENTATION_ITEM('Steel','Steel');
#7961=DESCRIPTIVE_REPRESENTATION_ITEM('Steel','Steel');
#7962=DESCRIPTIVE_REPRESENTATION_ITEM('Steel','Steel');
#7963=DESCRIPTIVE_REPRESENTATION_ITEM('Steel','Steel');
#7964=DESCRIPTIVE_REPRESENTATION_ITEM('Steel','Steel');
#7965=DESCRIPTIVE_REPRESENTATION_ITEM('Steel','Steel');
#7966=DESCRIPTIVE_REPRESENTATION_ITEM('Steel','Steel');
#7967=DESCRIPTIVE_REPRESENTATION_ITEM('Steel','Steel');
#7968=DESCRIPTIVE_REPRESENTATION_ITEM('Steel','Steel');
#7969=DESCRIPTIVE_REPRESENTATION_ITEM('Steel','Steel');
#7970=DESCRIPTIVE_REPRESENTATION_ITEM('Steel','Steel');
#7971=DESCRIPTIVE_REPRESENTATION_ITEM('Steel','Steel');
#7972=DESCRIPTIVE_REPRESENTATION_ITEM('Steel','Steel');
#7973=DESCRIPTIVE_REPRESENTATION_ITEM('Steel','Steel');
#7974=DESCRIPTIVE_REPRESENTATION_ITEM('Steel','Steel');
#7975=DESCRIPTIVE_REPRESENTATION_ITEM('Steel','Steel');
#7976=DESCRIPTIVE_REPRESENTATION_ITEM('Steel','Steel');
#7977=DESCRIPTIVE_REPRESENTATION_ITEM('Steel','Steel');
#7978=DESCRIPTIVE_REPRESENTATION_ITEM('Steel','Steel');
#7979=DESCRIPTIVE_REPRESENTATION_ITEM('Steel','Steel');
#7980=PROPERTY_DEFINITION('material property','material name',#14037);
#7981=PROPERTY_DEFINITION('material property','density of part',#14037);
#7982=PROPERTY_DEFINITION('material property','material name',#14038);
#7983=PROPERTY_DEFINITION('material property','density of part',#14038);
#7984=PROPERTY_DEFINITION('material property','material name',#14039);
#7985=PROPERTY_DEFINITION('material property','density of part',#14039);
#7986=PROPERTY_DEFINITION('material property','material name',#14040);
#7987=PROPERTY_DEFINITION('material property','density of part',#14040);
#7988=PROPERTY_DEFINITION('material property','material name',#14041);
#7989=PROPERTY_DEFINITION('material property','density of part',#14041);
#7990=PROPERTY_DEFINITION('material property','material name',#14042);
#7991=PROPERTY_DEFINITION('material property','density of part',#14042);
#7992=PROPERTY_DEFINITION('material property','material name',#14043);
#7993=PROPERTY_DEFINITION('material property','density of part',#14043);
#7994=PROPERTY_DEFINITION('material property','material name',#14044);
#7995=PROPERTY_DEFINITION('material property','density of part',#14044);
#7996=PROPERTY_DEFINITION('material property','material name',#14045);
#7997=PROPERTY_DEFINITION('material property','density of part',#14045);
#7998=PROPERTY_DEFINITION('material property','material name',#14046);
#7999=PROPERTY_DEFINITION('material property','density of part',#14046);
#8000=PROPERTY_DEFINITION('material property','material name',#14047);
#8001=PROPERTY_DEFINITION('material property','density of part',#14047);
#8002=PROPERTY_DEFINITION('material property','material name',#14048);
#8003=PROPERTY_DEFINITION('material property','density of part',#14048);
#8004=PROPERTY_DEFINITION('material property','material name',#14049);
#8005=PROPERTY_DEFINITION('material property','density of part',#14049);
#8006=PROPERTY_DEFINITION('material property','material name',#14050);
#8007=PROPERTY_DEFINITION('material property','density of part',#14050);
#8008=PROPERTY_DEFINITION('material property','material name',#14052);
#8009=PROPERTY_DEFINITION('material property','density of part',#14052);
#8010=PROPERTY_DEFINITION('material property','material name',#14053);
#8011=PROPERTY_DEFINITION('material property','density of part',#14053);
#8012=PROPERTY_DEFINITION('material property','material name',#14054);
#8013=PROPERTY_DEFINITION('material property','density of part',#14054);
#8014=PROPERTY_DEFINITION('material property','material name',#14055);
#8015=PROPERTY_DEFINITION('material property','density of part',#14055);
#8016=PROPERTY_DEFINITION('material property','material name',#14056);
#8017=PROPERTY_DEFINITION('material property','density of part',#14056);
#8018=PROPERTY_DEFINITION('material property','material name',#14057);
#8019=PROPERTY_DEFINITION('material property','density of part',#14057);
#8020=PROPERTY_DEFINITION('material property','material name',#14058);
#8021=PROPERTY_DEFINITION('material property','density of part',#14058);
#8022=PROPERTY_DEFINITION('material property','material name',#14059);
#8023=PROPERTY_DEFINITION('material property','density of part',#14059);
#8024=PROPERTY_DEFINITION('material property','material name',#14060);
#8025=PROPERTY_DEFINITION('material property','density of part',#14060);
#8026=PROPERTY_DEFINITION('material property','material name',#14062);
#8027=PROPERTY_DEFINITION('material property','density of part',#14062);
#8028=PROPERTY_DEFINITION('material property','material name',#14063);
#8029=PROPERTY_DEFINITION('material property','density of part',#14063);
#8030=PROPERTY_DEFINITION('material property','material name',#14064);
#8031=PROPERTY_DEFINITION('material property','density of part',#14064);
#8032=PROPERTY_DEFINITION('material property','material name',#14065);
#8033=PROPERTY_DEFINITION('material property','density of part',#14065);
#8034=PROPERTY_DEFINITION('material property','material name',#14066);
#8035=PROPERTY_DEFINITION('material property','density of part',#14066);
#8036=PROPERTY_DEFINITION('material property','material name',#14067);
#8037=PROPERTY_DEFINITION('material property','density of part',#14067);
#8038=PROPERTY_DEFINITION('material property','material name',#14068);
#8039=PROPERTY_DEFINITION('material property','density of part',#14068);
#8040=PROPERTY_DEFINITION('material property','material name',#14069);
#8041=PROPERTY_DEFINITION('material property','density of part',#14069);
#8042=PROPERTY_DEFINITION('material property','material name',#14070);
#8043=PROPERTY_DEFINITION('material property','density of part',#14070);
#8044=PROPERTY_DEFINITION('material property','material name',#14071);
#8045=PROPERTY_DEFINITION('material property','density of part',#14071);
#8046=PROPERTY_DEFINITION('material property','material name',#14072);
#8047=PROPERTY_DEFINITION('material property','density of part',#14072);
#8048=AXIS2_PLACEMENT_3D('',#11073,#8817,#8818);
#8049=AXIS2_PLACEMENT_3D('',#11074,#8819,#8820);
#8050=AXIS2_PLACEMENT_3D('',#11075,#8821,#8822);
#8051=AXIS2_PLACEMENT_3D('',#11076,#8823,#8824);
#8052=AXIS2_PLACEMENT_3D('',#11078,#8825,#8826);
#8053=AXIS2_PLACEMENT_3D('',#11081,#8828,#8829);
#8054=AXIS2_PLACEMENT_3D('',#11082,#8830,#8831);
#8055=AXIS2_PLACEMENT_3D('',#11084,#8832,#8833);
#8056=AXIS2_PLACEMENT_3D('',#11087,#8835,#8836);
#8057=AXIS2_PLACEMENT_3D('',#11088,#8837,#8838);
#8058=AXIS2_PLACEMENT_3D('',#11090,#8839,#8840);
#8059=AXIS2_PLACEMENT_3D('',#11093,#8842,#8843);
#8060=AXIS2_PLACEMENT_3D('',#11094,#8844,#8845);
#8061=AXIS2_PLACEMENT_3D('',#11096,#8846,#8847);
#8062=AXIS2_PLACEMENT_3D('',#11099,#8849,#8850);
#8063=AXIS2_PLACEMENT_3D('',#11100,#8851,#8852);
#8064=AXIS2_PLACEMENT_3D('',#11109,#8857,#8858);
#8065=AXIS2_PLACEMENT_3D('',#11115,#8862,#8863);
#8066=AXIS2_PLACEMENT_3D('',#11121,#8867,#8868);
#8067=AXIS2_PLACEMENT_3D('',#11124,#8871,#8872);
#8068=AXIS2_PLACEMENT_3D('',#11125,#8873,#8874);
#8069=AXIS2_PLACEMENT_3D('',#11126,#8875,#8876);
#8070=AXIS2_PLACEMENT_3D('',#11127,#8877,#8878);
#8071=AXIS2_PLACEMENT_3D('',#11129,#8879,#8880);
#8072=AXIS2_PLACEMENT_3D('',#11157,#8883,#8884);
#8073=AXIS2_PLACEMENT_3D('',#11229,#8885,#8886);
#8074=AXIS2_PLACEMENT_3D('',#11231,#8887,#8888);
#8075=AXIS2_PLACEMENT_3D('',#11233,#8890,#8891);
#8076=AXIS2_PLACEMENT_3D('',#11242,#8896,#8897);
#8077=AXIS2_PLACEMENT_3D('',#11248,#8901,#8902);
#8078=AXIS2_PLACEMENT_3D('',#11254,#8906,#8907);
#8079=AXIS2_PLACEMENT_3D('',#11260,#8911,#8912);
#8080=AXIS2_PLACEMENT_3D('',#11266,#8916,#8917);
#8081=AXIS2_PLACEMENT_3D('',#11272,#8921,#8922);
#8082=AXIS2_PLACEMENT_3D('',#11278,#8926,#8927);
#8083=AXIS2_PLACEMENT_3D('',#11284,#8931,#8932);
#8084=AXIS2_PLACEMENT_3D('',#11290,#8936,#8937);
#8085=AXIS2_PLACEMENT_3D('',#11299,#8942,#8943);
#8086=AXIS2_PLACEMENT_3D('',#11305,#8947,#8948);
#8087=AXIS2_PLACEMENT_3D('',#11311,#8952,#8953);
#8088=AXIS2_PLACEMENT_3D('',#11317,#8957,#8958);
#8089=AXIS2_PLACEMENT_3D('',#11323,#8962,#8963);
#8090=AXIS2_PLACEMENT_3D('',#11329,#8967,#8968);
#8091=AXIS2_PLACEMENT_3D('',#11335,#8972,#8973);
#8092=AXIS2_PLACEMENT_3D('',#11341,#8977,#8978);
#8093=AXIS2_PLACEMENT_3D('',#11347,#8982,#8983);
#8094=AXIS2_PLACEMENT_3D('',#11356,#8988,#8989);
#8095=AXIS2_PLACEMENT_3D('',#11362,#8993,#8994);
#8096=AXIS2_PLACEMENT_3D('',#11368,#8998,#8999);
#8097=AXIS2_PLACEMENT_3D('',#11374,#9003,#9004);
#8098=AXIS2_PLACEMENT_3D('',#11380,#9008,#9009);
#8099=AXIS2_PLACEMENT_3D('',#11386,#9013,#9014);
#8100=AXIS2_PLACEMENT_3D('',#11392,#9018,#9019);
#8101=AXIS2_PLACEMENT_3D('',#11398,#9023,#9024);
#8102=AXIS2_PLACEMENT_3D('',#11404,#9028,#9029);
#8103=AXIS2_PLACEMENT_3D('',#11413,#9034,#9035);
#8104=AXIS2_PLACEMENT_3D('',#11419,#9039,#9040);
#8105=AXIS2_PLACEMENT_3D('',#11425,#9044,#9045);
#8106=AXIS2_PLACEMENT_3D('',#11431,#9049,#9050);
#8107=AXIS2_PLACEMENT_3D('',#11437,#9054,#9055);
#8108=AXIS2_PLACEMENT_3D('',#11443,#9059,#9060);
#8109=AXIS2_PLACEMENT_3D('',#11449,#9064,#9065);
#8110=AXIS2_PLACEMENT_3D('',#11455,#9069,#9070);
#8111=AXIS2_PLACEMENT_3D('',#11461,#9074,#9075);
#8112=AXIS2_PLACEMENT_3D('',#11464,#9077,#9078);
#8113=AXIS2_PLACEMENT_3D('',#11465,#9079,#9080);
#8114=AXIS2_PLACEMENT_3D('',#11471,#9084,#9085);
#8115=AXIS2_PLACEMENT_3D('',#11477,#9089,#9090);
#8116=AXIS2_PLACEMENT_3D('',#11480,#9093,#9094);
#8117=AXIS2_PLACEMENT_3D('',#11486,#9098,#9099);
#8118=AXIS2_PLACEMENT_3D('',#11489,#9102,#9103);
#8119=AXIS2_PLACEMENT_3D('',#11495,#9107,#9108);
#8120=AXIS2_PLACEMENT_3D('',#11498,#9111,#9112);
#8121=AXIS2_PLACEMENT_3D('',#11501,#9115,#9116);
#8122=AXIS2_PLACEMENT_3D('',#11502,#9117,#9118);
#8123=AXIS2_PLACEMENT_3D('',#11503,#9119,#9120);
#8124=AXIS2_PLACEMENT_3D('',#11504,#9121,#9122);
#8125=AXIS2_PLACEMENT_3D('',#11506,#9123,#9124);
#8126=AXIS2_PLACEMENT_3D('',#11534,#9127,#9128);
#8127=AXIS2_PLACEMENT_3D('',#11606,#9129,#9130);
#8128=AXIS2_PLACEMENT_3D('',#11608,#9131,#9132);
#8129=AXIS2_PLACEMENT_3D('',#11610,#9134,#9135);
#8130=AXIS2_PLACEMENT_3D('',#11619,#9140,#9141);
#8131=AXIS2_PLACEMENT_3D('',#11625,#9145,#9146);
#8132=AXIS2_PLACEMENT_3D('',#11631,#9150,#9151);
#8133=AXIS2_PLACEMENT_3D('',#11637,#9155,#9156);
#8134=AXIS2_PLACEMENT_3D('',#11643,#9160,#9161);
#8135=AXIS2_PLACEMENT_3D('',#11649,#9165,#9166);
#8136=AXIS2_PLACEMENT_3D('',#11655,#9170,#9171);
#8137=AXIS2_PLACEMENT_3D('',#11661,#9175,#9176);
#8138=AXIS2_PLACEMENT_3D('',#11667,#9180,#9181);
#8139=AXIS2_PLACEMENT_3D('',#11676,#9186,#9187);
#8140=AXIS2_PLACEMENT_3D('',#11682,#9191,#9192);
#8141=AXIS2_PLACEMENT_3D('',#11688,#9196,#9197);
#8142=AXIS2_PLACEMENT_3D('',#11694,#9201,#9202);
#8143=AXIS2_PLACEMENT_3D('',#11700,#9206,#9207);
#8144=AXIS2_PLACEMENT_3D('',#11706,#9211,#9212);
#8145=AXIS2_PLACEMENT_3D('',#11712,#9216,#9217);
#8146=AXIS2_PLACEMENT_3D('',#11718,#9221,#9222);
#8147=AXIS2_PLACEMENT_3D('',#11724,#9226,#9227);
#8148=AXIS2_PLACEMENT_3D('',#11733,#9232,#9233);
#8149=AXIS2_PLACEMENT_3D('',#11739,#9237,#9238);
#8150=AXIS2_PLACEMENT_3D('',#11745,#9242,#9243);
#8151=AXIS2_PLACEMENT_3D('',#11751,#9247,#9248);
#8152=AXIS2_PLACEMENT_3D('',#11757,#9252,#9253);
#8153=AXIS2_PLACEMENT_3D('',#11763,#9257,#9258);
#8154=AXIS2_PLACEMENT_3D('',#11769,#9262,#9263);
#8155=AXIS2_PLACEMENT_3D('',#11775,#9267,#9268);
#8156=AXIS2_PLACEMENT_3D('',#11781,#9272,#9273);
#8157=AXIS2_PLACEMENT_3D('',#11790,#9278,#9279);
#8158=AXIS2_PLACEMENT_3D('',#11796,#9283,#9284);
#8159=AXIS2_PLACEMENT_3D('',#11802,#9288,#9289);
#8160=AXIS2_PLACEMENT_3D('',#11808,#9293,#9294);
#8161=AXIS2_PLACEMENT_3D('',#11814,#9298,#9299);
#8162=AXIS2_PLACEMENT_3D('',#11820,#9303,#9304);
#8163=AXIS2_PLACEMENT_3D('',#11826,#9308,#9309);
#8164=AXIS2_PLACEMENT_3D('',#11832,#9313,#9314);
#8165=AXIS2_PLACEMENT_3D('',#11838,#9318,#9319);
#8166=AXIS2_PLACEMENT_3D('',#11841,#9321,#9322);
#8167=AXIS2_PLACEMENT_3D('',#11842,#9323,#9324);
#8168=AXIS2_PLACEMENT_3D('',#11848,#9328,#9329);
#8169=AXIS2_PLACEMENT_3D('',#11854,#9333,#9334);
#8170=AXIS2_PLACEMENT_3D('',#11857,#9337,#9338);
#8171=AXIS2_PLACEMENT_3D('',#11863,#9342,#9343);
#8172=AXIS2_PLACEMENT_3D('',#11866,#9346,#9347);
#8173=AXIS2_PLACEMENT_3D('',#11872,#9351,#9352);
#8174=AXIS2_PLACEMENT_3D('',#11875,#9355,#9356);
#8175=AXIS2_PLACEMENT_3D('',#11878,#9359,#9360);
#8176=AXIS2_PLACEMENT_3D('',#11879,#9361,#9362);
#8177=AXIS2_PLACEMENT_3D('',#11880,#9363,#9364);
#8178=AXIS2_PLACEMENT_3D('',#11881,#9365,#9366);
#8179=AXIS2_PLACEMENT_3D('',#11890,#9371,#9372);
#8180=AXIS2_PLACEMENT_3D('',#11896,#9376,#9377);
#8181=AXIS2_PLACEMENT_3D('',#11902,#9381,#9382);
#8182=AXIS2_PLACEMENT_3D('',#11908,#9386,#9387);
#8183=AXIS2_PLACEMENT_3D('',#11914,#9391,#9392);
#8184=AXIS2_PLACEMENT_3D('',#11920,#9396,#9397);
#8185=AXIS2_PLACEMENT_3D('',#11926,#9401,#9402);
#8186=AXIS2_PLACEMENT_3D('',#11932,#9406,#9407);
#8187=AXIS2_PLACEMENT_3D('',#11938,#9411,#9412);
#8188=AXIS2_PLACEMENT_3D('',#11947,#9417,#9418);
#8189=AXIS2_PLACEMENT_3D('',#11953,#9422,#9423);
#8190=AXIS2_PLACEMENT_3D('',#11959,#9427,#9428);
#8191=AXIS2_PLACEMENT_3D('',#11965,#9432,#9433);
#8192=AXIS2_PLACEMENT_3D('',#11971,#9437,#9438);
#8193=AXIS2_PLACEMENT_3D('',#11977,#9442,#9443);
#8194=AXIS2_PLACEMENT_3D('',#11983,#9447,#9448);
#8195=AXIS2_PLACEMENT_3D('',#11989,#9452,#9453);
#8196=AXIS2_PLACEMENT_3D('',#11995,#9457,#9458);
#8197=AXIS2_PLACEMENT_3D('',#12004,#9463,#9464);
#8198=AXIS2_PLACEMENT_3D('',#12010,#9468,#9469);
#8199=AXIS2_PLACEMENT_3D('',#12016,#9473,#9474);
#8200=AXIS2_PLACEMENT_3D('',#12022,#9478,#9479);
#8201=AXIS2_PLACEMENT_3D('',#12028,#9483,#9484);
#8202=AXIS2_PLACEMENT_3D('',#12034,#9488,#9489);
#8203=AXIS2_PLACEMENT_3D('',#12040,#9493,#9494);
#8204=AXIS2_PLACEMENT_3D('',#12046,#9498,#9499);
#8205=AXIS2_PLACEMENT_3D('',#12052,#9503,#9504);
#8206=AXIS2_PLACEMENT_3D('',#12061,#9509,#9510);
#8207=AXIS2_PLACEMENT_3D('',#12067,#9514,#9515);
#8208=AXIS2_PLACEMENT_3D('',#12073,#9519,#9520);
#8209=AXIS2_PLACEMENT_3D('',#12079,#9524,#9525);
#8210=AXIS2_PLACEMENT_3D('',#12085,#9529,#9530);
#8211=AXIS2_PLACEMENT_3D('',#12091,#9534,#9535);
#8212=AXIS2_PLACEMENT_3D('',#12097,#9539,#9540);
#8213=AXIS2_PLACEMENT_3D('',#12103,#9544,#9545);
#8214=AXIS2_PLACEMENT_3D('',#12109,#9549,#9550);
#8215=AXIS2_PLACEMENT_3D('',#12111,#9551,#9552);
#8216=AXIS2_PLACEMENT_3D('',#12114,#9554,#9555);
#8217=AXIS2_PLACEMENT_3D('',#12115,#9556,#9557);
#8218=AXIS2_PLACEMENT_3D('',#12121,#9561,#9562);
#8219=AXIS2_PLACEMENT_3D('',#12127,#9566,#9567);
#8220=AXIS2_PLACEMENT_3D('',#12130,#9570,#9571);
#8221=AXIS2_PLACEMENT_3D('',#12136,#9575,#9576);
#8222=AXIS2_PLACEMENT_3D('',#12139,#9579,#9580);
#8223=AXIS2_PLACEMENT_3D('',#12145,#9584,#9585);
#8224=AXIS2_PLACEMENT_3D('',#12148,#9588,#9589);
#8225=AXIS2_PLACEMENT_3D('',#12151,#9592,#9593);
#8226=AXIS2_PLACEMENT_3D('',#12152,#9594,#9595);
#8227=AXIS2_PLACEMENT_3D('',#12153,#9596,#9597);
#8228=AXIS2_PLACEMENT_3D('',#12154,#9598,#9599);
#8229=AXIS2_PLACEMENT_3D('',#12163,#9604,#9605);
#8230=AXIS2_PLACEMENT_3D('',#12169,#9609,#9610);
#8231=AXIS2_PLACEMENT_3D('',#12175,#9614,#9615);
#8232=AXIS2_PLACEMENT_3D('',#12181,#9619,#9620);
#8233=AXIS2_PLACEMENT_3D('',#12187,#9624,#9625);
#8234=AXIS2_PLACEMENT_3D('',#12190,#9628,#9629);
#8235=AXIS2_PLACEMENT_3D('',#12191,#9630,#9631);
#8236=AXIS2_PLACEMENT_3D('',#12192,#9632,#9633);
#8237=AXIS2_PLACEMENT_3D('',#12194,#9634,#9635);
#8238=AXIS2_PLACEMENT_3D('',#12196,#9636,#9637);
#8239=AXIS2_PLACEMENT_3D('',#12197,#9638,#9639);
#8240=AXIS2_PLACEMENT_3D('',#12200,#9641,#9642);
#8241=AXIS2_PLACEMENT_3D('',#12201,#9643,#9644);
#8242=AXIS2_PLACEMENT_3D('',#12202,#9645,#9646);
#8243=AXIS2_PLACEMENT_3D('',#12204,#9647,#9648);
#8244=AXIS2_PLACEMENT_3D('',#12205,#9649,#9650);
#8245=AXIS2_PLACEMENT_3D('',#12207,#9651,#9652);
#8246=AXIS2_PLACEMENT_3D('',#12209,#9654,#9655);
#8247=AXIS2_PLACEMENT_3D('',#12211,#9656,#9657);
#8248=AXIS2_PLACEMENT_3D('',#12213,#9659,#9660);
#8249=AXIS2_PLACEMENT_3D('',#12215,#9661,#9662);
#8250=AXIS2_PLACEMENT_3D('',#12217,#9664,#9665);
#8251=AXIS2_PLACEMENT_3D('',#12219,#9666,#9667);
#8252=AXIS2_PLACEMENT_3D('',#12220,#9668,#9669);
#8253=AXIS2_PLACEMENT_3D('',#12222,#9670,#9671);
#8254=AXIS2_PLACEMENT_3D('',#12224,#9673,#9674);
#8255=AXIS2_PLACEMENT_3D('',#12226,#9676,#9677);
#8256=AXIS2_PLACEMENT_3D('',#12227,#9678,#9679);
#8257=AXIS2_PLACEMENT_3D('',#12229,#9680,#9681);
#8258=AXIS2_PLACEMENT_3D('',#12230,#9682,#9683);
#8259=AXIS2_PLACEMENT_3D('',#12232,#9684,#9685);
#8260=AXIS2_PLACEMENT_3D('',#12234,#9687,#9688);
#8261=AXIS2_PLACEMENT_3D('',#12236,#9689,#9690);
#8262=AXIS2_PLACEMENT_3D('',#12238,#9692,#9693);
#8263=AXIS2_PLACEMENT_3D('',#12240,#9694,#9695);
#8264=AXIS2_PLACEMENT_3D('',#12242,#9697,#9698);
#8265=AXIS2_PLACEMENT_3D('',#12244,#9699,#9700);
#8266=AXIS2_PLACEMENT_3D('',#12245,#9701,#9702);
#8267=AXIS2_PLACEMENT_3D('',#12247,#9703,#9704);
#8268=AXIS2_PLACEMENT_3D('',#12249,#9706,#9707);
#8269=AXIS2_PLACEMENT_3D('',#12251,#9708,#9709);
#8270=AXIS2_PLACEMENT_3D('',#12253,#9711,#9712);
#8271=AXIS2_PLACEMENT_3D('',#12255,#9713,#9714);
#8272=AXIS2_PLACEMENT_3D('',#12257,#9716,#9717);
#8273=AXIS2_PLACEMENT_3D('',#12258,#9718,#9719);
#8274=AXIS2_PLACEMENT_3D('',#12267,#9724,#9725);
#8275=AXIS2_PLACEMENT_3D('',#12273,#9729,#9730);
#8276=AXIS2_PLACEMENT_3D('',#12279,#9734,#9735);
#8277=AXIS2_PLACEMENT_3D('',#12285,#9739,#9740);
#8278=AXIS2_PLACEMENT_3D('',#12291,#9744,#9745);
#8279=AXIS2_PLACEMENT_3D('',#12294,#9748,#9749);
#8280=AXIS2_PLACEMENT_3D('',#12295,#9750,#9751);
#8281=AXIS2_PLACEMENT_3D('',#12296,#9752,#9753);
#8282=AXIS2_PLACEMENT_3D('',#12297,#9754,#9755);
#8283=AXIS2_PLACEMENT_3D('',#12299,#9756,#9757);
#8284=AXIS2_PLACEMENT_3D('',#12302,#9759,#9760);
#8285=AXIS2_PLACEMENT_3D('',#12303,#9761,#9762);
#8286=AXIS2_PLACEMENT_3D('',#12305,#9763,#9764);
#8287=AXIS2_PLACEMENT_3D('',#12308,#9766,#9767);
#8288=AXIS2_PLACEMENT_3D('',#12309,#9768,#9769);
#8289=AXIS2_PLACEMENT_3D('',#12311,#9770,#9771);
#8290=AXIS2_PLACEMENT_3D('',#12314,#9773,#9774);
#8291=AXIS2_PLACEMENT_3D('',#12315,#9775,#9776);
#8292=AXIS2_PLACEMENT_3D('',#12317,#9777,#9778);
#8293=AXIS2_PLACEMENT_3D('',#12320,#9780,#9781);
#8294=AXIS2_PLACEMENT_3D('',#12321,#9782,#9783);
#8295=AXIS2_PLACEMENT_3D('',#12330,#9788,#9789);
#8296=AXIS2_PLACEMENT_3D('',#12336,#9793,#9794);
#8297=AXIS2_PLACEMENT_3D('',#12342,#9798,#9799);
#8298=AXIS2_PLACEMENT_3D('',#12345,#9802,#9803);
#8299=AXIS2_PLACEMENT_3D('',#12346,#9804,#9805);
#8300=AXIS2_PLACEMENT_3D('',#12347,#9806,#9807);
#8301=AXIS2_PLACEMENT_3D('',#12348,#9808,#9809);
#8302=AXIS2_PLACEMENT_3D('',#12350,#9810,#9811);
#8303=AXIS2_PLACEMENT_3D('',#12353,#9813,#9814);
#8304=AXIS2_PLACEMENT_3D('',#12354,#9815,#9816);
#8305=AXIS2_PLACEMENT_3D('',#12357,#9818,#9819);
#8306=AXIS2_PLACEMENT_3D('',#12358,#9820,#9821);
#8307=AXIS2_PLACEMENT_3D('',#12360,#9822,#9823);
#8308=AXIS2_PLACEMENT_3D('',#12361,#9824,#9825);
#8309=AXIS2_PLACEMENT_3D('',#12364,#9827,#9828);
#8310=AXIS2_PLACEMENT_3D('',#12365,#9829,#9830);
#8311=AXIS2_PLACEMENT_3D('',#12366,#9831,#9832);
#8312=AXIS2_PLACEMENT_3D('',#12367,#9833,#9834);
#8313=AXIS2_PLACEMENT_3D('',#12369,#9835,#9836);
#8314=AXIS2_PLACEMENT_3D('',#12372,#9838,#9839);
#8315=AXIS2_PLACEMENT_3D('',#12373,#9840,#9841);
#8316=AXIS2_PLACEMENT_3D('',#12375,#9842,#9843);
#8317=AXIS2_PLACEMENT_3D('',#12378,#9845,#9846);
#8318=AXIS2_PLACEMENT_3D('',#12379,#9847,#9848);
#8319=AXIS2_PLACEMENT_3D('',#12388,#9853,#9854);
#8320=AXIS2_PLACEMENT_3D('',#12394,#9858,#9859);
#8321=AXIS2_PLACEMENT_3D('',#12400,#9863,#9864);
#8322=AXIS2_PLACEMENT_3D('',#12403,#9867,#9868);
#8323=AXIS2_PLACEMENT_3D('',#12404,#9869,#9870);
#8324=AXIS2_PLACEMENT_3D('',#12405,#9871,#9872);
#8325=AXIS2_PLACEMENT_3D('',#12406,#9873,#9874);
#8326=AXIS2_PLACEMENT_3D('',#12415,#9879,#9880);
#8327=AXIS2_PLACEMENT_3D('',#12421,#9884,#9885);
#8328=AXIS2_PLACEMENT_3D('',#12427,#9889,#9890);
#8329=AXIS2_PLACEMENT_3D('',#12430,#9893,#9894);
#8330=AXIS2_PLACEMENT_3D('',#12431,#9895,#9896);
#8331=AXIS2_PLACEMENT_3D('',#12432,#9897,#9898);
#8332=AXIS2_PLACEMENT_3D('',#12433,#9899,#9900);
#8333=AXIS2_PLACEMENT_3D('',#12442,#9905,#9906);
#8334=AXIS2_PLACEMENT_3D('',#12448,#9910,#9911);
#8335=AXIS2_PLACEMENT_3D('',#12454,#9915,#9916);
#8336=AXIS2_PLACEMENT_3D('',#12457,#9919,#9920);
#8337=AXIS2_PLACEMENT_3D('',#12458,#9921,#9922);
#8338=AXIS2_PLACEMENT_3D('',#12459,#9923,#9924);
#8339=AXIS2_PLACEMENT_3D('',#12460,#9925,#9926);
#8340=AXIS2_PLACEMENT_3D('',#12462,#9927,#9928);
#8341=AXIS2_PLACEMENT_3D('',#12465,#9930,#9931);
#8342=AXIS2_PLACEMENT_3D('',#12466,#9932,#9933);
#8343=AXIS2_PLACEMENT_3D('',#12468,#9934,#9935);
#8344=AXIS2_PLACEMENT_3D('',#12471,#9937,#9938);
#8345=AXIS2_PLACEMENT_3D('',#12472,#9939,#9940);
#8346=AXIS2_PLACEMENT_3D('',#12481,#9945,#9946);
#8347=AXIS2_PLACEMENT_3D('',#12487,#9950,#9951);
#8348=AXIS2_PLACEMENT_3D('',#12493,#9955,#9956);
#8349=AXIS2_PLACEMENT_3D('',#12496,#9959,#9960);
#8350=AXIS2_PLACEMENT_3D('',#12497,#9961,#9962);
#8351=AXIS2_PLACEMENT_3D('',#12498,#9963,#9964);
#8352=AXIS2_PLACEMENT_3D('',#12499,#9965,#9966);
#8353=AXIS2_PLACEMENT_3D('',#12508,#9971,#9972);
#8354=AXIS2_PLACEMENT_3D('',#12514,#9976,#9977);
#8355=AXIS2_PLACEMENT_3D('',#12520,#9981,#9982);
#8356=AXIS2_PLACEMENT_3D('',#12523,#9985,#9986);
#8357=AXIS2_PLACEMENT_3D('',#12524,#9987,#9988);
#8358=AXIS2_PLACEMENT_3D('',#12525,#9989,#9990);
#8359=AXIS2_PLACEMENT_3D('',#12526,#9991,#9992);
#8360=AXIS2_PLACEMENT_3D('',#12535,#9997,#9998);
#8361=AXIS2_PLACEMENT_3D('',#12541,#10002,#10003);
#8362=AXIS2_PLACEMENT_3D('',#12547,#10007,#10008);
#8363=AXIS2_PLACEMENT_3D('',#12550,#10011,#10012);
#8364=AXIS2_PLACEMENT_3D('',#12551,#10013,#10014);
#8365=AXIS2_PLACEMENT_3D('',#12552,#10015,#10016);
#8366=AXIS2_PLACEMENT_3D('',#12553,#10017,#10018);
#8367=AXIS2_PLACEMENT_3D('',#12554,#10019,#10020);
#8368=AXIS2_PLACEMENT_3D('',#12556,#10021,#10022);
#8369=AXIS2_PLACEMENT_3D('',#12559,#10024,#10025);
#8370=AXIS2_PLACEMENT_3D('',#12560,#10026,#10027);
#8371=AXIS2_PLACEMENT_3D('',#12562,#10028,#10029);
#8372=AXIS2_PLACEMENT_3D('',#12565,#10031,#10032);
#8373=AXIS2_PLACEMENT_3D('',#12566,#10033,#10034);
#8374=AXIS2_PLACEMENT_3D('',#12567,#10035,#10036);
#8375=AXIS2_PLACEMENT_3D('',#12568,#10037,#10038);
#8376=AXIS2_PLACEMENT_3D('',#12569,#10039,#10040);
#8377=AXIS2_PLACEMENT_3D('',#12571,#10041,#10042);
#8378=AXIS2_PLACEMENT_3D('',#12574,#10044,#10045);
#8379=AXIS2_PLACEMENT_3D('',#12575,#10046,#10047);
#8380=AXIS2_PLACEMENT_3D('',#12577,#10048,#10049);
#8381=AXIS2_PLACEMENT_3D('',#12578,#10050,#10051);
#8382=AXIS2_PLACEMENT_3D('',#12581,#10053,#10054);
#8383=AXIS2_PLACEMENT_3D('',#12582,#10055,#10056);
#8384=AXIS2_PLACEMENT_3D('',#12584,#10057,#10058);
#8385=AXIS2_PLACEMENT_3D('',#12587,#10060,#10061);
#8386=AXIS2_PLACEMENT_3D('',#12588,#10062,#10063);
#8387=AXIS2_PLACEMENT_3D('',#12589,#10064,#10065);
#8388=AXIS2_PLACEMENT_3D('',#12590,#10066,#10067);
#8389=AXIS2_PLACEMENT_3D('',#12591,#10068,#10069);
#8390=AXIS2_PLACEMENT_3D('',#12593,#10070,#10071);
#8391=AXIS2_PLACEMENT_3D('',#12596,#10073,#10074);
#8392=AXIS2_PLACEMENT_3D('',#12597,#10075,#10076);
#8393=AXIS2_PLACEMENT_3D('',#12599,#10077,#10078);
#8394=AXIS2_PLACEMENT_3D('',#12600,#10079,#10080);
#8395=AXIS2_PLACEMENT_3D('',#12603,#10082,#10083);
#8396=AXIS2_PLACEMENT_3D('',#12604,#10084,#10085);
#8397=AXIS2_PLACEMENT_3D('',#12606,#10086,#10087);
#8398=AXIS2_PLACEMENT_3D('',#12609,#10089,#10090);
#8399=AXIS2_PLACEMENT_3D('',#12610,#10091,#10092);
#8400=AXIS2_PLACEMENT_3D('',#12611,#10093,#10094);
#8401=AXIS2_PLACEMENT_3D('',#12612,#10095,#10096);
#8402=AXIS2_PLACEMENT_3D('',#12613,#10097,#10098);
#8403=AXIS2_PLACEMENT_3D('',#12615,#10099,#10100);
#8404=AXIS2_PLACEMENT_3D('',#12618,#10102,#10103);
#8405=AXIS2_PLACEMENT_3D('',#12619,#10104,#10105);
#8406=AXIS2_PLACEMENT_3D('',#12621,#10106,#10107);
#8407=AXIS2_PLACEMENT_3D('',#12622,#10108,#10109);
#8408=AXIS2_PLACEMENT_3D('',#12624,#10110,#10111);
#8409=AXIS2_PLACEMENT_3D('',#12626,#10113,#10114);
#8410=AXIS2_PLACEMENT_3D('',#12628,#10115,#10116);
#8411=AXIS2_PLACEMENT_3D('',#12631,#10118,#10119);
#8412=AXIS2_PLACEMENT_3D('',#12632,#10120,#10121);
#8413=AXIS2_PLACEMENT_3D('',#12633,#10122,#10123);
#8414=AXIS2_PLACEMENT_3D('',#12634,#10124,#10125);
#8415=AXIS2_PLACEMENT_3D('',#12635,#10126,#10127);
#8416=AXIS2_PLACEMENT_3D('',#12637,#10128,#10129);
#8417=AXIS2_PLACEMENT_3D('',#12640,#10131,#10132);
#8418=AXIS2_PLACEMENT_3D('',#12641,#10133,#10134);
#8419=AXIS2_PLACEMENT_3D('',#12643,#10135,#10136);
#8420=AXIS2_PLACEMENT_3D('',#12644,#10137,#10138);
#8421=AXIS2_PLACEMENT_3D('',#12646,#10139,#10140);
#8422=AXIS2_PLACEMENT_3D('',#12648,#10142,#10143);
#8423=AXIS2_PLACEMENT_3D('',#12650,#10144,#10145);
#8424=AXIS2_PLACEMENT_3D('',#12653,#10147,#10148);
#8425=AXIS2_PLACEMENT_3D('',#12654,#10149,#10150);
#8426=AXIS2_PLACEMENT_3D('',#12655,#10151,#10152);
#8427=AXIS2_PLACEMENT_3D('',#12656,#10153,#10154);
#8428=AXIS2_PLACEMENT_3D('',#12657,#10155,#10156);
#8429=AXIS2_PLACEMENT_3D('',#12659,#10157,#10158);
#8430=AXIS2_PLACEMENT_3D('',#12662,#10160,#10161);
#8431=AXIS2_PLACEMENT_3D('',#12663,#10162,#10163);
#8432=AXIS2_PLACEMENT_3D('',#12664,#10164,#10165);
#8433=AXIS2_PLACEMENT_3D('',#12666,#10166,#10167);
#8434=AXIS2_PLACEMENT_3D('',#12669,#10169,#10170);
#8435=AXIS2_PLACEMENT_3D('',#12670,#10171,#10172);
#8436=AXIS2_PLACEMENT_3D('',#12671,#10173,#10174);
#8437=AXIS2_PLACEMENT_3D('',#12673,#10175,#10176);
#8438=AXIS2_PLACEMENT_3D('',#12676,#10178,#10179);
#8439=AXIS2_PLACEMENT_3D('',#12677,#10180,#10181);
#8440=AXIS2_PLACEMENT_3D('',#12678,#10182,#10183);
#8441=AXIS2_PLACEMENT_3D('',#12679,#10184,#10185);
#8442=AXIS2_PLACEMENT_3D('',#12680,#10186,#10187);
#8443=AXIS2_PLACEMENT_3D('',#12682,#10188,#10189);
#8444=AXIS2_PLACEMENT_3D('',#12685,#10191,#10192);
#8445=AXIS2_PLACEMENT_3D('',#12686,#10193,#10194);
#8446=AXIS2_PLACEMENT_3D('',#12688,#10195,#10196);
#8447=AXIS2_PLACEMENT_3D('',#12689,#10197,#10198);
#8448=AXIS2_PLACEMENT_3D('',#12691,#10199,#10200);
#8449=AXIS2_PLACEMENT_3D('',#12694,#10202,#10203);
#8450=AXIS2_PLACEMENT_3D('',#12695,#10204,#10205);
#8451=AXIS2_PLACEMENT_3D('',#12697,#10206,#10207);
#8452=AXIS2_PLACEMENT_3D('',#12698,#10208,#10209);
#8453=AXIS2_PLACEMENT_3D('',#12700,#10210,#10211);
#8454=AXIS2_PLACEMENT_3D('',#12702,#10213,#10214);
#8455=AXIS2_PLACEMENT_3D('',#12704,#10215,#10216);
#8456=AXIS2_PLACEMENT_3D('',#12706,#10218,#10219);
#8457=AXIS2_PLACEMENT_3D('',#12708,#10220,#10221);
#8458=AXIS2_PLACEMENT_3D('',#12711,#10223,#10224);
#8459=AXIS2_PLACEMENT_3D('',#12712,#10225,#10226);
#8460=AXIS2_PLACEMENT_3D('',#12721,#10231,#10232);
#8461=AXIS2_PLACEMENT_3D('',#12727,#10236,#10237);
#8462=AXIS2_PLACEMENT_3D('',#12733,#10241,#10242);
#8463=AXIS2_PLACEMENT_3D('',#12736,#10245,#10246);
#8464=AXIS2_PLACEMENT_3D('',#12737,#10247,#10248);
#8465=AXIS2_PLACEMENT_3D('',#12738,#10249,#10250);
#8466=AXIS2_PLACEMENT_3D('',#12739,#10251,#10252);
#8467=AXIS2_PLACEMENT_3D('',#12741,#10253,#10254);
#8468=AXIS2_PLACEMENT_3D('',#12744,#10256,#10257);
#8469=AXIS2_PLACEMENT_3D('',#12745,#10258,#10259);
#8470=AXIS2_PLACEMENT_3D('',#12747,#10260,#10261);
#8471=AXIS2_PLACEMENT_3D('',#12750,#10263,#10264);
#8472=AXIS2_PLACEMENT_3D('',#12751,#10265,#10266);
#8473=AXIS2_PLACEMENT_3D('',#12752,#10267,#10268);
#8474=AXIS2_PLACEMENT_3D('',#12753,#10269,#10270);
#8475=AXIS2_PLACEMENT_3D('',#12754,#10271,#10272);
#8476=AXIS2_PLACEMENT_3D('',#12756,#10273,#10274);
#8477=AXIS2_PLACEMENT_3D('',#12759,#10276,#10277);
#8478=AXIS2_PLACEMENT_3D('',#12760,#10278,#10279);
#8479=AXIS2_PLACEMENT_3D('',#12762,#10280,#10281);
#8480=AXIS2_PLACEMENT_3D('',#12765,#10283,#10284);
#8481=AXIS2_PLACEMENT_3D('',#12766,#10285,#10286);
#8482=AXIS2_PLACEMENT_3D('',#12767,#10287,#10288);
#8483=AXIS2_PLACEMENT_3D('',#12768,#10289,#10290);
#8484=AXIS2_PLACEMENT_3D('',#12769,#10291,#10292);
#8485=AXIS2_PLACEMENT_3D('',#12770,#10293,#10294);
#8486=AXIS2_PLACEMENT_3D('',#12773,#10295,#10296);
#8487=AXIS2_PLACEMENT_3D('',#12774,#10297,#10298);
#8488=AXIS2_PLACEMENT_3D('',#12776,#10299,#10300);
#8489=AXIS2_PLACEMENT_3D('',#12778,#10301,#10302);
#8490=AXIS2_PLACEMENT_3D('',#12779,#10303,#10304);
#8491=AXIS2_PLACEMENT_3D('',#12780,#10305,#10306);
#8492=AXIS2_PLACEMENT_3D('',#12783,#10308,#10309);
#8493=AXIS2_PLACEMENT_3D('',#12784,#10310,#10311);
#8494=AXIS2_PLACEMENT_3D('',#12786,#10312,#10313);
#8495=AXIS2_PLACEMENT_3D('',#12789,#10315,#10316);
#8496=AXIS2_PLACEMENT_3D('',#12790,#10317,#10318);
#8497=AXIS2_PLACEMENT_3D('',#12793,#10320,#10321);
#8498=AXIS2_PLACEMENT_3D('',#12794,#10322,#10323);
#8499=AXIS2_PLACEMENT_3D('',#12795,#10324,#10325);
#8500=AXIS2_PLACEMENT_3D('',#12797,#10326,#10327);
#8501=AXIS2_PLACEMENT_3D('',#12799,#10329,#10330);
#8502=AXIS2_PLACEMENT_3D('',#12801,#10331,#10332);
#8503=AXIS2_PLACEMENT_3D('',#12802,#10333,#10334);
#8504=AXIS2_PLACEMENT_3D('',#12804,#10336,#10337);
#8505=AXIS2_PLACEMENT_3D('',#12805,#10338,#10339);
#8506=AXIS2_PLACEMENT_3D('',#12808,#10340,#10341);
#8507=AXIS2_PLACEMENT_3D('',#12809,#10342,#10343);
#8508=AXIS2_PLACEMENT_3D('',#12811,#10344,#10345);
#8509=AXIS2_PLACEMENT_3D('',#12813,#10346,#10347);
#8510=AXIS2_PLACEMENT_3D('',#12814,#10348,#10349);
#8511=AXIS2_PLACEMENT_3D('',#12815,#10350,#10351);
#8512=AXIS2_PLACEMENT_3D('',#12817,#10352,#10353);
#8513=AXIS2_PLACEMENT_3D('',#12819,#10355,#10356);
#8514=AXIS2_PLACEMENT_3D('',#12821,#10357,#10358);
#8515=AXIS2_PLACEMENT_3D('',#12823,#10359,#10360);
#8516=AXIS2_PLACEMENT_3D('',#12824,#10361,#10362);
#8517=AXIS2_PLACEMENT_3D('',#12826,#10363,#10364);
#8518=AXIS2_PLACEMENT_3D('',#12828,#10366,#10367);
#8519=AXIS2_PLACEMENT_3D('',#12830,#10368,#10369);
#8520=AXIS2_PLACEMENT_3D('',#12832,#10371,#10372);
#8521=AXIS2_PLACEMENT_3D('',#12834,#10373,#10374);
#8522=AXIS2_PLACEMENT_3D('',#12836,#10376,#10377);
#8523=AXIS2_PLACEMENT_3D('',#12837,#10378,#10379);
#8524=AXIS2_PLACEMENT_3D('',#12839,#10381,#10382);
#8525=AXIS2_PLACEMENT_3D('',#12840,#10383,#10384);
#8526=AXIS2_PLACEMENT_3D('',#12843,#10385,#10386);
#8527=AXIS2_PLACEMENT_3D('',#12844,#10387,#10388);
#8528=AXIS2_PLACEMENT_3D('',#12847,#10389,#10390);
#8529=AXIS2_PLACEMENT_3D('',#12848,#10391,#10392);
#8530=AXIS2_PLACEMENT_3D('',#12851,#10393,#10394);
#8531=AXIS2_PLACEMENT_3D('',#12852,#10395,#10396);
#8532=AXIS2_PLACEMENT_3D('',#12855,#10397,#10398);
#8533=AXIS2_PLACEMENT_3D('',#12856,#10399,#10400);
#8534=AXIS2_PLACEMENT_3D('',#12859,#10401,#10402);
#8535=AXIS2_PLACEMENT_3D('',#12860,#10403,#10404);
#8536=AXIS2_PLACEMENT_3D('',#12863,#10405,#10406);
#8537=AXIS2_PLACEMENT_3D('',#12864,#10407,#10408);
#8538=AXIS2_PLACEMENT_3D('',#12867,#10409,#10410);
#8539=AXIS2_PLACEMENT_3D('',#12868,#10411,#10412);
#8540=AXIS2_PLACEMENT_3D('',#12871,#10413,#10414);
#8541=AXIS2_PLACEMENT_3D('',#12872,#10415,#10416);
#8542=AXIS2_PLACEMENT_3D('',#12873,#10417,#10418);
#8543=AXIS2_PLACEMENT_3D('',#12899,#10419,#10420);
#8544=AXIS2_PLACEMENT_3D('',#12923,#10421,#10422);
#8545=AXIS2_PLACEMENT_3D('',#12924,#10423,#10424);
#8546=AXIS2_PLACEMENT_3D('',#12926,#10425,#10426);
#8547=AXIS2_PLACEMENT_3D('',#12951,#10427,#10428);
#8548=AXIS2_PLACEMENT_3D('',#12976,#10429,#10430);
#8549=AXIS2_PLACEMENT_3D('',#12992,#10432,#10433);
#8550=AXIS2_PLACEMENT_3D('',#13007,#10434,#10435);
#8551=AXIS2_PLACEMENT_3D('',#13032,#10436,#10437);
#8552=AXIS2_PLACEMENT_3D('',#13057,#10438,#10439);
#8553=AXIS2_PLACEMENT_3D('',#13082,#10440,#10441);
#8554=AXIS2_PLACEMENT_3D('',#13106,#10442,#10443);
#8555=AXIS2_PLACEMENT_3D('',#13107,#10444,#10445);
#8556=AXIS2_PLACEMENT_3D('',#13109,#10446,#10447);
#8557=AXIS2_PLACEMENT_3D('',#13110,#10448,#10449);
#8558=AXIS2_PLACEMENT_3D('',#13111,#10450,#10451);
#8559=AXIS2_PLACEMENT_3D('',#13135,#10452,#10453);
#8560=AXIS2_PLACEMENT_3D('',#13136,#10454,#10455);
#8561=AXIS2_PLACEMENT_3D('',#13138,#10456,#10457);
#8562=AXIS2_PLACEMENT_3D('',#13139,#10458,#10459);
#8563=AXIS2_PLACEMENT_3D('',#13140,#10460,#10461);
#8564=AXIS2_PLACEMENT_3D('',#13164,#10462,#10463);
#8565=AXIS2_PLACEMENT_3D('',#13165,#10464,#10465);
#8566=AXIS2_PLACEMENT_3D('',#13167,#10466,#10467);
#8567=AXIS2_PLACEMENT_3D('',#13168,#10468,#10469);
#8568=AXIS2_PLACEMENT_3D('',#13169,#10470,#10471);
#8569=AXIS2_PLACEMENT_3D('',#13184,#10472,#10473);
#8570=AXIS2_PLACEMENT_3D('',#13197,#10474,#10475);
#8571=AXIS2_PLACEMENT_3D('',#13199,#10476,#10477);
#8572=AXIS2_PLACEMENT_3D('',#13200,#10478,#10479);
#8573=AXIS2_PLACEMENT_3D('',#13201,#10480,#10481);
#8574=AXIS2_PLACEMENT_3D('',#13225,#10482,#10483);
#8575=AXIS2_PLACEMENT_3D('',#13226,#10484,#10485);
#8576=AXIS2_PLACEMENT_3D('',#13228,#10486,#10487);
#8577=AXIS2_PLACEMENT_3D('',#13229,#10488,#10489);
#8578=AXIS2_PLACEMENT_3D('',#13230,#10490,#10491);
#8579=AXIS2_PLACEMENT_3D('',#13254,#10492,#10493);
#8580=AXIS2_PLACEMENT_3D('',#13255,#10494,#10495);
#8581=AXIS2_PLACEMENT_3D('',#13257,#10496,#10497);
#8582=AXIS2_PLACEMENT_3D('',#13258,#10498,#10499);
#8583=AXIS2_PLACEMENT_3D('',#13259,#10500,#10501);
#8584=AXIS2_PLACEMENT_3D('',#13283,#10502,#10503);
#8585=AXIS2_PLACEMENT_3D('',#13284,#10504,#10505);
#8586=AXIS2_PLACEMENT_3D('',#13286,#10506,#10507);
#8587=AXIS2_PLACEMENT_3D('',#13289,#10509,#10510);
#8588=AXIS2_PLACEMENT_3D('',#13313,#10511,#10512);
#8589=AXIS2_PLACEMENT_3D('',#13314,#10513,#10514);
#8590=AXIS2_PLACEMENT_3D('',#13315,#10515,#10516);
#8591=AXIS2_PLACEMENT_3D('',#13316,#10517,#10518);
#8592=AXIS2_PLACEMENT_3D('',#13317,#10519,#10520);
#8593=AXIS2_PLACEMENT_3D('',#13318,#10521,#10522);
#8594=AXIS2_PLACEMENT_3D('',#13319,#10523,#10524);
#8595=AXIS2_PLACEMENT_3D('',#13320,#10525,#10526);
#8596=AXIS2_PLACEMENT_3D('',#13321,#10527,#10528);
#8597=AXIS2_PLACEMENT_3D('',#13323,#10529,#10530);
#8598=AXIS2_PLACEMENT_3D('',#13325,#10531,#10532);
#8599=AXIS2_PLACEMENT_3D('',#13326,#10533,#10534);
#8600=AXIS2_PLACEMENT_3D('',#13328,#10535,#10536);
#8601=AXIS2_PLACEMENT_3D('',#13330,#10538,#10539);
#8602=AXIS2_PLACEMENT_3D('',#13332,#10540,#10541);
#8603=AXIS2_PLACEMENT_3D('',#13333,#10542,#10543);
#8604=AXIS2_PLACEMENT_3D('',#13335,#10545,#10546);
#8605=AXIS2_PLACEMENT_3D('',#13337,#10547,#10548);
#8606=AXIS2_PLACEMENT_3D('',#13339,#10549,#10550);
#8607=AXIS2_PLACEMENT_3D('',#13340,#10551,#10552);
#8608=AXIS2_PLACEMENT_3D('',#13342,#10553,#10554);
#8609=AXIS2_PLACEMENT_3D('',#13344,#10556,#10557);
#8610=AXIS2_PLACEMENT_3D('',#13346,#10558,#10559);
#8611=AXIS2_PLACEMENT_3D('',#13347,#10560,#10561);
#8612=AXIS2_PLACEMENT_3D('',#13349,#10563,#10564);
#8613=AXIS2_PLACEMENT_3D('',#13350,#10565,#10566);
#8614=AXIS2_PLACEMENT_3D('',#13351,#10567,#10568);
#8615=AXIS2_PLACEMENT_3D('',#13352,#10569,#10570);
#8616=AXIS2_PLACEMENT_3D('',#13353,#10571,#10572);
#8617=AXIS2_PLACEMENT_3D('',#13354,#10573,#10574);
#8618=AXIS2_PLACEMENT_3D('',#13355,#10575,#10576);
#8619=AXIS2_PLACEMENT_3D('',#13357,#10577,#10578);
#8620=AXIS2_PLACEMENT_3D('',#13360,#10580,#10581);
#8621=AXIS2_PLACEMENT_3D('',#13361,#10582,#10583);
#8622=AXIS2_PLACEMENT_3D('',#13363,#10584,#10585);
#8623=AXIS2_PLACEMENT_3D('',#13366,#10587,#10588);
#8624=AXIS2_PLACEMENT_3D('',#13367,#10589,#10590);
#8625=AXIS2_PLACEMENT_3D('',#13368,#10591,#10592);
#8626=AXIS2_PLACEMENT_3D('',#13369,#10593,#10594);
#8627=AXIS2_PLACEMENT_3D('',#13370,#10595,#10596);
#8628=AXIS2_PLACEMENT_3D('',#13379,#10601,#10602);
#8629=AXIS2_PLACEMENT_3D('',#13385,#10606,#10607);
#8630=AXIS2_PLACEMENT_3D('',#13391,#10611,#10612);
#8631=AXIS2_PLACEMENT_3D('',#13397,#10616,#10617);
#8632=AXIS2_PLACEMENT_3D('',#13403,#10621,#10622);
#8633=AXIS2_PLACEMENT_3D('',#13406,#10625,#10626);
#8634=AXIS2_PLACEMENT_3D('',#13407,#10627,#10628);
#8635=AXIS2_PLACEMENT_3D('',#13408,#10629,#10630);
#8636=AXIS2_PLACEMENT_3D('',#13410,#10631,#10632);
#8637=AXIS2_PLACEMENT_3D('',#13411,#10633,#10634);
#8638=AXIS2_PLACEMENT_3D('',#13413,#10635,#10636);
#8639=AXIS2_PLACEMENT_3D('',#13414,#10637,#10638);
#8640=AXIS2_PLACEMENT_3D('',#13416,#10639,#10640);
#8641=AXIS2_PLACEMENT_3D('',#13418,#10642,#10643);
#8642=AXIS2_PLACEMENT_3D('',#13420,#10644,#10645);
#8643=AXIS2_PLACEMENT_3D('',#13422,#10647,#10648);
#8644=AXIS2_PLACEMENT_3D('',#13424,#10649,#10650);
#8645=AXIS2_PLACEMENT_3D('',#13426,#10652,#10653);
#8646=AXIS2_PLACEMENT_3D('',#13428,#10654,#10655);
#8647=AXIS2_PLACEMENT_3D('',#13429,#10656,#10657);
#8648=AXIS2_PLACEMENT_3D('',#13431,#10658,#10659);
#8649=AXIS2_PLACEMENT_3D('',#13433,#10661,#10662);
#8650=AXIS2_PLACEMENT_3D('',#13435,#10664,#10665);
#8651=AXIS2_PLACEMENT_3D('',#13436,#10666,#10667);
#8652=AXIS2_PLACEMENT_3D('',#13438,#10668,#10669);
#8653=AXIS2_PLACEMENT_3D('',#13441,#10671,#10672);
#8654=AXIS2_PLACEMENT_3D('',#13442,#10673,#10674);
#8655=AXIS2_PLACEMENT_3D('',#13444,#10675,#10676);
#8656=AXIS2_PLACEMENT_3D('',#13447,#10678,#10679);
#8657=AXIS2_PLACEMENT_3D('',#13448,#10680,#10681);
#8658=AXIS2_PLACEMENT_3D('',#13449,#10682,#10683);
#8659=AXIS2_PLACEMENT_3D('',#13450,#10684,#10685);
#8660=AXIS2_PLACEMENT_3D('',#13451,#10686,#10687);
#8661=AXIS2_PLACEMENT_3D('',#13460,#10692,#10693);
#8662=AXIS2_PLACEMENT_3D('',#13466,#10697,#10698);
#8663=AXIS2_PLACEMENT_3D('',#13473,#10702,#10703);
#8664=AXIS2_PLACEMENT_3D('',#13474,#10704,#10705);
#8665=AXIS2_PLACEMENT_3D('',#13488,#10713,#10714);
#8666=AXIS2_PLACEMENT_3D('',#13492,#10717,#10718);
#8667=AXIS2_PLACEMENT_3D('',#13496,#10721,#10722);
#8668=AXIS2_PLACEMENT_3D('',#13506,#10728,#10729);
#8669=AXIS2_PLACEMENT_3D('',#13508,#10731,#10732);
#8670=AXIS2_PLACEMENT_3D('',#13512,#10734,#10735);
#8671=AXIS2_PLACEMENT_3D('',#13514,#10737,#10738);
#8672=AXIS2_PLACEMENT_3D('',#13516,#10739,#10740);
#8673=AXIS2_PLACEMENT_3D('',#13519,#10742,#10743);
#8674=AXIS2_PLACEMENT_3D('',#13521,#10744,#10745);
#8675=AXIS2_PLACEMENT_3D('',#13522,#10746,#10747);
#8676=AXIS2_PLACEMENT_3D('',#13523,#10748,#10749);
#8677=AXIS2_PLACEMENT_3D('',#13525,#10751,#10752);
#8678=AXIS2_PLACEMENT_3D('',#13527,#10754,#10755);
#8679=AXIS2_PLACEMENT_3D('',#13529,#10757,#10758);
#8680=AXIS2_PLACEMENT_3D('',#13530,#10759,#10760);
#8681=AXIS2_PLACEMENT_3D('',#13531,#10761,#10762);
#8682=AXIS2_PLACEMENT_3D('',#13540,#10767,#10768);
#8683=AXIS2_PLACEMENT_3D('',#13546,#10772,#10773);
#8684=AXIS2_PLACEMENT_3D('',#13552,#10777,#10778);
#8685=AXIS2_PLACEMENT_3D('',#13558,#10782,#10783);
#8686=AXIS2_PLACEMENT_3D('',#13564,#10787,#10788);
#8687=AXIS2_PLACEMENT_3D('',#13567,#10791,#10792);
#8688=AXIS2_PLACEMENT_3D('',#13568,#10793,#10794);
#8689=AXIS2_PLACEMENT_3D('',#13569,#10795,#10796);
#8690=AXIS2_PLACEMENT_3D('',#13571,#10797,#10798);
#8691=AXIS2_PLACEMENT_3D('',#13572,#10799,#10800);
#8692=AXIS2_PLACEMENT_3D('',#13574,#10801,#10802);
#8693=AXIS2_PLACEMENT_3D('',#13575,#10803,#10804);
#8694=AXIS2_PLACEMENT_3D('',#13577,#10805,#10806);
#8695=AXIS2_PLACEMENT_3D('',#13579,#10808,#10809);
#8696=AXIS2_PLACEMENT_3D('',#13581,#10810,#10811);
#8697=AXIS2_PLACEMENT_3D('',#13583,#10813,#10814);
#8698=AXIS2_PLACEMENT_3D('',#13585,#10815,#10816);
#8699=AXIS2_PLACEMENT_3D('',#13587,#10818,#10819);
#8700=AXIS2_PLACEMENT_3D('',#13589,#10820,#10821);
#8701=AXIS2_PLACEMENT_3D('',#13590,#10822,#10823);
#8702=AXIS2_PLACEMENT_3D('',#13592,#10824,#10825);
#8703=AXIS2_PLACEMENT_3D('',#13594,#10827,#10828);
#8704=AXIS2_PLACEMENT_3D('',#13596,#10830,#10831);
#8705=AXIS2_PLACEMENT_3D('',#13597,#10832,#10833);
#8706=AXIS2_PLACEMENT_3D('',#13598,#10834,#10835);
#8707=AXIS2_PLACEMENT_3D('',#13599,#10836,#10837);
#8708=AXIS2_PLACEMENT_3D('',#13600,#10838,#10839);
#8709=AXIS2_PLACEMENT_3D('',#13601,#10840,#10841);
#8710=AXIS2_PLACEMENT_3D('',#13602,#10842,#10843);
#8711=AXIS2_PLACEMENT_3D('',#13603,#10844,#10845);
#8712=AXIS2_PLACEMENT_3D('',#13604,#10846,#10847);
#8713=AXIS2_PLACEMENT_3D('',#13605,#10848,#10849);
#8714=AXIS2_PLACEMENT_3D('',#13606,#10850,#10851);
#8715=AXIS2_PLACEMENT_3D('',#13607,#10852,#10853);
#8716=AXIS2_PLACEMENT_3D('',#13608,#10854,#10855);
#8717=AXIS2_PLACEMENT_3D('',#13609,#10856,#10857);
#8718=AXIS2_PLACEMENT_3D('',#13610,#10858,#10859);
#8719=AXIS2_PLACEMENT_3D('',#13611,#10860,#10861);
#8720=AXIS2_PLACEMENT_3D('',#13612,#10862,#10863);
#8721=AXIS2_PLACEMENT_3D('',#13613,#10864,#10865);
#8722=AXIS2_PLACEMENT_3D('',#13614,#10866,#10867);
#8723=AXIS2_PLACEMENT_3D('',#13615,#10868,#10869);
#8724=AXIS2_PLACEMENT_3D('',#13616,#10870,#10871);
#8725=AXIS2_PLACEMENT_3D('',#13617,#10872,#10873);
#8726=AXIS2_PLACEMENT_3D('',#13618,#10874,#10875);
#8727=AXIS2_PLACEMENT_3D('',#13619,#10876,#10877);
#8728=AXIS2_PLACEMENT_3D('',#13620,#10878,#10879);
#8729=AXIS2_PLACEMENT_3D('',#13621,#10880,#10881);
#8730=AXIS2_PLACEMENT_3D('',#13622,#10882,#10883);
#8731=AXIS2_PLACEMENT_3D('',#13623,#10884,#10885);
#8732=AXIS2_PLACEMENT_3D('',#13624,#10886,#10887);
#8733=AXIS2_PLACEMENT_3D('',#13625,#10888,#10889);
#8734=AXIS2_PLACEMENT_3D('',#13626,#10890,#10891);
#8735=AXIS2_PLACEMENT_3D('',#13627,#10892,#10893);
#8736=AXIS2_PLACEMENT_3D('',#13628,#10894,#10895);
#8737=AXIS2_PLACEMENT_3D('',#13629,#10896,#10897);
#8738=AXIS2_PLACEMENT_3D('',#13630,#10898,#10899);
#8739=AXIS2_PLACEMENT_3D('',#13631,#10900,#10901);
#8740=AXIS2_PLACEMENT_3D('',#13632,#10902,#10903);
#8741=AXIS2_PLACEMENT_3D('',#13633,#10904,#10905);
#8742=AXIS2_PLACEMENT_3D('',#13634,#10906,#10907);
#8743=AXIS2_PLACEMENT_3D('',#13635,#10908,#10909);
#8744=AXIS2_PLACEMENT_3D('',#13636,#10910,#10911);
#8745=AXIS2_PLACEMENT_3D('',#13637,#10912,#10913);
#8746=AXIS2_PLACEMENT_3D('',#13638,#10914,#10915);
#8747=AXIS2_PLACEMENT_3D('',#13639,#10916,#10917);
#8748=AXIS2_PLACEMENT_3D('',#13640,#10918,#10919);
#8749=AXIS2_PLACEMENT_3D('',#13641,#10920,#10921);
#8750=AXIS2_PLACEMENT_3D('',#13642,#10922,#10923);
#8751=AXIS2_PLACEMENT_3D('',#13643,#10924,#10925);
#8752=AXIS2_PLACEMENT_3D('',#13644,#10926,#10927);
#8753=AXIS2_PLACEMENT_3D('',#13645,#10928,#10929);
#8754=AXIS2_PLACEMENT_3D('',#13646,#10930,#10931);
#8755=AXIS2_PLACEMENT_3D('',#13647,#10932,#10933);
#8756=AXIS2_PLACEMENT_3D('',#13648,#10934,#10935);
#8757=AXIS2_PLACEMENT_3D('',#13649,#10936,#10937);
#8758=AXIS2_PLACEMENT_3D('',#13650,#10938,#10939);
#8759=AXIS2_PLACEMENT_3D('',#13651,#10940,#10941);
#8760=AXIS2_PLACEMENT_3D('',#13652,#10942,#10943);
#8761=AXIS2_PLACEMENT_3D('',#13653,#10944,#10945);
#8762=AXIS2_PLACEMENT_3D('',#13655,#10946,#10947);
#8763=AXIS2_PLACEMENT_3D('',#13658,#10949,#10950);
#8764=AXIS2_PLACEMENT_3D('',#13659,#10951,#10952);
#8765=AXIS2_PLACEMENT_3D('',#13661,#10953,#10954);
#8766=AXIS2_PLACEMENT_3D('',#13662,#10955,#10956);
#8767=AXIS2_PLACEMENT_3D('',#13664,#10957,#10958);
#8768=AXIS2_PLACEMENT_3D('',#13667,#10960,#10961);
#8769=AXIS2_PLACEMENT_3D('',#13668,#10962,#10963);
#8770=AXIS2_PLACEMENT_3D('',#13670,#10964,#10965);
#8771=AXIS2_PLACEMENT_3D('',#13671,#10966,#10967);
#8772=AXIS2_PLACEMENT_3D('',#13673,#10968,#10969);
#8773=AXIS2_PLACEMENT_3D('',#13675,#10971,#10972);
#8774=AXIS2_PLACEMENT_3D('',#13677,#10973,#10974);
#8775=AXIS2_PLACEMENT_3D('',#13679,#10976,#10977);
#8776=AXIS2_PLACEMENT_3D('',#13681,#10978,#10979);
#8777=AXIS2_PLACEMENT_3D('',#13684,#10981,#10982);
#8778=AXIS2_PLACEMENT_3D('',#13685,#10983,#10984);
#8779=AXIS2_PLACEMENT_3D('',#13694,#10989,#10990);
#8780=AXIS2_PLACEMENT_3D('',#13700,#10994,#10995);
#8781=AXIS2_PLACEMENT_3D('',#13706,#10999,#11000);
#8782=AXIS2_PLACEMENT_3D('',#13709,#11003,#11004);
#8783=AXIS2_PLACEMENT_3D('',#13710,#11005,#11006);
#8784=AXIS2_PLACEMENT_3D('',#13711,#11007,#11008);
#8785=AXIS2_PLACEMENT_3D('',#13712,#11009,#11010);
#8786=AXIS2_PLACEMENT_3D('',#13713,#11011,#11012);
#8787=AXIS2_PLACEMENT_3D('',#13714,#11013,#11014);
#8788=AXIS2_PLACEMENT_3D('',#13715,#11015,#11016);
#8789=AXIS2_PLACEMENT_3D('',#13716,#11017,#11018);
#8790=AXIS2_PLACEMENT_3D('',#13717,#11019,#11020);
#8791=AXIS2_PLACEMENT_3D('',#13718,#11021,#11022);
#8792=AXIS2_PLACEMENT_3D('',#13719,#11023,#11024);
#8793=AXIS2_PLACEMENT_3D('',#13720,#11025,#11026);
#8794=AXIS2_PLACEMENT_3D('',#13721,#11027,#11028);
#8795=AXIS2_PLACEMENT_3D('',#13722,#11029,#11030);
#8796=AXIS2_PLACEMENT_3D('',#13723,#11031,#11032);
#8797=AXIS2_PLACEMENT_3D('',#13724,#11033,#11034);
#8798=AXIS2_PLACEMENT_3D('',#13725,#11035,#11036);
#8799=AXIS2_PLACEMENT_3D('',#13726,#11037,#11038);
#8800=AXIS2_PLACEMENT_3D('',#13727,#11039,#11040);
#8801=AXIS2_PLACEMENT_3D('',#13728,#11041,#11042);
#8802=AXIS2_PLACEMENT_3D('',#13729,#11043,#11044);
#8803=AXIS2_PLACEMENT_3D('',#13730,#11045,#11046);
#8804=AXIS2_PLACEMENT_3D('',#13731,#11047,#11048);
#8805=AXIS2_PLACEMENT_3D('',#13732,#11049,#11050);
#8806=AXIS2_PLACEMENT_3D('',#13733,#11051,#11052);
#8807=AXIS2_PLACEMENT_3D('',#13734,#11053,#11054);
#8808=AXIS2_PLACEMENT_3D('',#13735,#11055,#11056);
#8809=AXIS2_PLACEMENT_3D('',#13736,#11057,#11058);
#8810=AXIS2_PLACEMENT_3D('',#13737,#11059,#11060);
#8811=AXIS2_PLACEMENT_3D('',#13738,#11061,#11062);
#8812=AXIS2_PLACEMENT_3D('',#13739,#11063,#11064);
#8813=AXIS2_PLACEMENT_3D('',#13740,#11065,#11066);
#8814=AXIS2_PLACEMENT_3D('',#13741,#11067,#11068);
#8815=AXIS2_PLACEMENT_3D('',#13742,#11069,#11070);
#8816=AXIS2_PLACEMENT_3D('',#13743,#11071,#11072);
#8817=DIRECTION('axis',(0.,0.,1.));
#8818=DIRECTION('refdir',(1.,0.,0.));
#8819=DIRECTION('axis',(0.,0.,1.));
#8820=DIRECTION('refdir',(1.,0.,0.));
#8821=DIRECTION('axis',(0.,0.,1.));
#8822=DIRECTION('refdir',(1.,0.,0.));
#8823=DIRECTION('center_axis',(0.,1.,0.));
#8824=DIRECTION('ref_axis',(1.,0.,0.));
#8825=DIRECTION('center_axis',(0.,1.,0.));
#8826=DIRECTION('ref_axis',(1.,0.,0.));
#8827=DIRECTION('',(0.,1.,0.));
#8828=DIRECTION('center_axis',(0.,-1.,0.));
#8829=DIRECTION('ref_axis',(1.,0.,0.));
#8830=DIRECTION('center_axis',(0.,1.,0.));
#8831=DIRECTION('ref_axis',(1.,0.,0.));
#8832=DIRECTION('center_axis',(0.,1.,0.));
#8833=DIRECTION('ref_axis',(1.,0.,0.));
#8834=DIRECTION('',(0.,1.,0.));
#8835=DIRECTION('center_axis',(0.,-1.,0.));
#8836=DIRECTION('ref_axis',(1.,0.,0.));
#8837=DIRECTION('center_axis',(0.,1.,0.));
#8838=DIRECTION('ref_axis',(1.,0.,0.));
#8839=DIRECTION('center_axis',(0.,1.,0.));
#8840=DIRECTION('ref_axis',(1.,0.,0.));
#8841=DIRECTION('',(0.,1.,0.));
#8842=DIRECTION('center_axis',(0.,-1.,0.));
#8843=DIRECTION('ref_axis',(1.,0.,0.));
#8844=DIRECTION('center_axis',(0.,1.,0.));
#8845=DIRECTION('ref_axis',(1.,0.,0.));
#8846=DIRECTION('center_axis',(0.,1.,0.));
#8847=DIRECTION('ref_axis',(1.,0.,0.));
#8848=DIRECTION('',(0.,1.,0.));
#8849=DIRECTION('center_axis',(0.,-1.,0.));
#8850=DIRECTION('ref_axis',(1.,0.,0.));
#8851=DIRECTION('center_axis',(0.,1.,0.));
#8852=DIRECTION('ref_axis',(-1.,0.,0.));
#8853=DIRECTION('',(-1.,0.,0.));
#8854=DIRECTION('',(0.,0.,1.));
#8855=DIRECTION('',(-1.,0.,0.));
#8856=DIRECTION('',(0.,0.,1.));
#8857=DIRECTION('center_axis',(1.,0.,0.));
#8858=DIRECTION('ref_axis',(0.,1.,0.));
#8859=DIRECTION('',(0.,1.,0.));
#8860=DIRECTION('',(0.,1.,0.));
#8861=DIRECTION('',(0.,0.,1.));
#8862=DIRECTION('center_axis',(0.,-1.,0.));
#8863=DIRECTION('ref_axis',(1.,0.,0.));
#8864=DIRECTION('',(1.,0.,0.));
#8865=DIRECTION('',(1.,0.,0.));
#8866=DIRECTION('',(0.,0.,1.));
#8867=DIRECTION('center_axis',(-1.,0.,0.));
#8868=DIRECTION('ref_axis',(0.,-1.,0.));
#8869=DIRECTION('',(0.,-1.,0.));
#8870=DIRECTION('',(0.,-1.,0.));
#8871=DIRECTION('center_axis',(0.,0.,1.));
#8872=DIRECTION('ref_axis',(1.,0.,0.));
#8873=DIRECTION('center_axis',(0.,0.,1.));
#8874=DIRECTION('ref_axis',(1.,0.,0.));
#8875=DIRECTION('axis',(0.,0.,1.));
#8876=DIRECTION('refdir',(1.,0.,0.));
#8877=DIRECTION('center_axis',(0.,0.,1.));
#8878=DIRECTION('ref_axis',(1.,0.,0.));
#8879=DIRECTION('center_axis',(0.,0.,1.));
#8880=DIRECTION('ref_axis',(1.,0.,0.));
#8881=DIRECTION('',(0.,0.,1.));
#8882=DIRECTION('',(0.,0.,1.));
#8883=DIRECTION('center_axis',(0.,0.,-1.));
#8884=DIRECTION('ref_axis',(1.,0.,0.));
#8885=DIRECTION('center_axis',(1.,0.,0.));
#8886=DIRECTION('ref_axis',(0.,0.,-1.));
#8887=DIRECTION('center_axis',(1.,0.,0.));
#8888=DIRECTION('ref_axis',(0.,0.,-1.));
#8889=DIRECTION('',(1.,0.,0.));
#8890=DIRECTION('center_axis',(0.,0.,-1.));
#8891=DIRECTION('ref_axis',(0.,1.,0.));
#8892=DIRECTION('',(0.,1.,0.));
#8893=DIRECTION('',(1.,0.,0.));
#8894=DIRECTION('',(0.,-1.,0.));
#8895=DIRECTION('',(1.,0.,0.));
#8896=DIRECTION('center_axis',(0.,1.,-8.88178419700125E-16));
#8897=DIRECTION('ref_axis',(0.,8.88178419700125E-16,1.));
#8898=DIRECTION('',(0.,8.88178419700125E-16,1.));
#8899=DIRECTION('',(1.,0.,0.));
#8900=DIRECTION('',(0.,-8.88178419700125E-16,-1.));
#8901=DIRECTION('center_axis',(0.,-7.40148683083439E-16,-1.));
#8902=DIRECTION('ref_axis',(0.,1.,-7.40148683083439E-16));
#8903=DIRECTION('',(0.,1.,-7.40148683083439E-16));
#8904=DIRECTION('',(1.,0.,0.));
#8905=DIRECTION('',(0.,-1.,7.40148683083439E-16));
#8906=DIRECTION('center_axis',(0.,-0.707106781186547,-0.707106781186548));
#8907=DIRECTION('ref_axis',(0.,0.707106781186548,-0.707106781186547));
#8908=DIRECTION('',(0.,0.707106781186548,-0.707106781186547));
#8909=DIRECTION('',(1.,0.,0.));
#8910=DIRECTION('',(0.,-0.707106781186548,0.707106781186547));
#8911=DIRECTION('center_axis',(0.,-1.,2.77555756156289E-16));
#8912=DIRECTION('ref_axis',(0.,-2.77555756156289E-16,-1.));
#8913=DIRECTION('',(0.,-2.77555756156289E-16,-1.));
#8914=DIRECTION('',(1.,0.,0.));
#8915=DIRECTION('',(0.,2.77555756156289E-16,1.));
#8916=DIRECTION('center_axis',(0.,-0.707106781186547,0.707106781186548));
#8917=DIRECTION('ref_axis',(0.,-0.707106781186548,-0.707106781186547));
#8918=DIRECTION('',(0.,-0.707106781186548,-0.707106781186547));
#8919=DIRECTION('',(1.,0.,0.));
#8920=DIRECTION('',(0.,0.707106781186548,0.707106781186547));
#8921=DIRECTION('center_axis',(0.,7.40148683083438E-16,1.));
#8922=DIRECTION('ref_axis',(0.,-1.,7.40148683083438E-16));
#8923=DIRECTION('',(0.,-1.,7.40148683083438E-16));
#8924=DIRECTION('',(1.,0.,0.));
#8925=DIRECTION('',(0.,1.,-7.40148683083438E-16));
#8926=DIRECTION('center_axis',(0.,1.,-4.44089209850063E-16));
#8927=DIRECTION('ref_axis',(0.,4.44089209850063E-16,1.));
#8928=DIRECTION('',(0.,4.44089209850063E-16,1.));
#8929=DIRECTION('',(1.,0.,0.));
#8930=DIRECTION('',(0.,-4.44089209850063E-16,-1.));
#8931=DIRECTION('center_axis',(0.,2.41352831440251E-16,1.));
#8932=DIRECTION('ref_axis',(0.,-1.,2.41352831440251E-16));
#8933=DIRECTION('',(0.,-1.,2.41352831440251E-16));
#8934=DIRECTION('',(-1.,0.,0.));
#8935=DIRECTION('',(0.,1.,-2.41352831440251E-16));
#8936=DIRECTION('center_axis',(0.,-1.,2.41352831440251E-16));
#8937=DIRECTION('ref_axis',(0.,-2.41352831440251E-16,-1.));
#8938=DIRECTION('',(0.,-2.41352831440251E-16,-1.));
#8939=DIRECTION('',(1.,0.,0.));
#8940=DIRECTION('',(0.,2.41352831440251E-16,1.));
#8941=DIRECTION('',(1.,0.,0.));
#8942=DIRECTION('center_axis',(0.,0.,-1.));
#8943=DIRECTION('ref_axis',(0.,1.,0.));
#8944=DIRECTION('',(0.,1.,0.));
#8945=DIRECTION('',(1.,0.,0.));
#8946=DIRECTION('',(0.,-1.,0.));
#8947=DIRECTION('center_axis',(0.,-1.,0.));
#8948=DIRECTION('ref_axis',(0.,0.,-1.));
#8949=DIRECTION('',(0.,0.,-1.));
#8950=DIRECTION('',(1.,0.,0.));
#8951=DIRECTION('',(0.,0.,1.));
#8952=DIRECTION('center_axis',(0.,-0.707106781186547,0.707106781186548));
#8953=DIRECTION('ref_axis',(0.,-0.707106781186548,-0.707106781186547));
#8954=DIRECTION('',(0.,-0.707106781186548,-0.707106781186547));
#8955=DIRECTION('',(1.,0.,0.));
#8956=DIRECTION('',(0.,0.707106781186548,0.707106781186547));
#8957=DIRECTION('center_axis',(0.,0.,1.));
#8958=DIRECTION('ref_axis',(0.,-1.,0.));
#8959=DIRECTION('',(0.,-1.,0.));
#8960=DIRECTION('',(1.,0.,0.));
#8961=DIRECTION('',(0.,1.,0.));
#8962=DIRECTION('center_axis',(0.,0.707106781186548,0.707106781186547));
#8963=DIRECTION('ref_axis',(0.,-0.707106781186547,0.707106781186548));
#8964=DIRECTION('',(0.,-0.707106781186547,0.707106781186548));
#8965=DIRECTION('',(1.,0.,0.));
#8966=DIRECTION('',(0.,0.707106781186547,-0.707106781186548));
#8967=DIRECTION('center_axis',(0.,1.,0.));
#8968=DIRECTION('ref_axis',(0.,0.,1.));
#8969=DIRECTION('',(0.,0.,1.));
#8970=DIRECTION('',(1.,0.,0.));
#8971=DIRECTION('',(0.,0.,-1.));
#8972=DIRECTION('center_axis',(0.,0.,-1.));
#8973=DIRECTION('ref_axis',(0.,1.,0.));
#8974=DIRECTION('',(0.,1.,0.));
#8975=DIRECTION('',(1.,0.,0.));
#8976=DIRECTION('',(0.,-1.,0.));
#8977=DIRECTION('center_axis',(0.,1.,-2.41352831440251E-16));
#8978=DIRECTION('ref_axis',(0.,2.41352831440251E-16,1.));
#8979=DIRECTION('',(0.,2.41352831440251E-16,1.));
#8980=DIRECTION('',(-1.,0.,0.));
#8981=DIRECTION('',(0.,-2.41352831440251E-16,-1.));
#8982=DIRECTION('center_axis',(0.,0.,1.));
#8983=DIRECTION('ref_axis',(0.,-1.,0.));
#8984=DIRECTION('',(0.,-1.,0.));
#8985=DIRECTION('',(1.,0.,0.));
#8986=DIRECTION('',(0.,1.,0.));
#8987=DIRECTION('',(1.,0.,0.));
#8988=DIRECTION('center_axis',(0.,-1.,0.));
#8989=DIRECTION('ref_axis',(0.,0.,-1.));
#8990=DIRECTION('',(0.,0.,-1.));
#8991=DIRECTION('',(1.,0.,0.));
#8992=DIRECTION('',(0.,0.,1.));
#8993=DIRECTION('center_axis',(0.,0.,1.));
#8994=DIRECTION('ref_axis',(0.,-1.,0.));
#8995=DIRECTION('',(0.,-1.,0.));
#8996=DIRECTION('',(1.,0.,0.));
#8997=DIRECTION('',(0.,1.,0.));
#8998=DIRECTION('center_axis',(0.,0.707106781186548,0.707106781186548));
#8999=DIRECTION('ref_axis',(0.,-0.707106781186548,0.707106781186548));
#9000=DIRECTION('',(0.,-0.707106781186548,0.707106781186548));
#9001=DIRECTION('',(1.,0.,0.));
#9002=DIRECTION('',(0.,0.707106781186548,-0.707106781186548));
#9003=DIRECTION('center_axis',(0.,1.,0.));
#9004=DIRECTION('ref_axis',(0.,0.,1.));
#9005=DIRECTION('',(0.,0.,1.));
#9006=DIRECTION('',(1.,0.,0.));
#9007=DIRECTION('',(0.,0.,-1.));
#9008=DIRECTION('center_axis',(0.,0.707106781186548,-0.707106781186547));
#9009=DIRECTION('ref_axis',(0.,0.707106781186547,0.707106781186548));
#9010=DIRECTION('',(0.,0.707106781186547,0.707106781186548));
#9011=DIRECTION('',(1.,0.,0.));
#9012=DIRECTION('',(0.,-0.707106781186547,-0.707106781186548));
#9013=DIRECTION('center_axis',(0.,-7.40148683083438E-16,-1.));
#9014=DIRECTION('ref_axis',(0.,1.,-7.40148683083438E-16));
#9015=DIRECTION('',(0.,1.,-7.40148683083438E-16));
#9016=DIRECTION('',(1.,0.,0.));
#9017=DIRECTION('',(0.,-1.,7.40148683083438E-16));
#9018=DIRECTION('center_axis',(0.,-1.,0.));
#9019=DIRECTION('ref_axis',(0.,0.,-1.));
#9020=DIRECTION('',(0.,0.,-1.));
#9021=DIRECTION('',(1.,0.,0.));
#9022=DIRECTION('',(0.,0.,1.));
#9023=DIRECTION('center_axis',(0.,0.,-1.));
#9024=DIRECTION('ref_axis',(0.,1.,0.));
#9025=DIRECTION('',(0.,1.,0.));
#9026=DIRECTION('',(-1.,0.,0.));
#9027=DIRECTION('',(0.,-1.,0.));
#9028=DIRECTION('center_axis',(0.,1.,0.));
#9029=DIRECTION('ref_axis',(0.,0.,1.));
#9030=DIRECTION('',(0.,0.,1.));
#9031=DIRECTION('',(1.,0.,0.));
#9032=DIRECTION('',(0.,0.,-1.));
#9033=DIRECTION('',(1.,0.,0.));
#9034=DIRECTION('center_axis',(0.,0.,1.));
#9035=DIRECTION('ref_axis',(0.,-1.,0.));
#9036=DIRECTION('',(0.,-1.,0.));
#9037=DIRECTION('',(1.,0.,0.));
#9038=DIRECTION('',(0.,1.,0.));
#9039=DIRECTION('center_axis',(0.,1.,0.));
#9040=DIRECTION('ref_axis',(0.,0.,1.));
#9041=DIRECTION('',(0.,0.,1.));
#9042=DIRECTION('',(1.,0.,0.));
#9043=DIRECTION('',(0.,0.,-1.));
#9044=DIRECTION('center_axis',(0.,0.707106781186547,-0.707106781186548));
#9045=DIRECTION('ref_axis',(0.,0.707106781186548,0.707106781186547));
#9046=DIRECTION('',(0.,0.707106781186548,0.707106781186547));
#9047=DIRECTION('',(1.,0.,0.));
#9048=DIRECTION('',(0.,-0.707106781186548,-0.707106781186547));
#9049=DIRECTION('center_axis',(0.,0.,-1.));
#9050=DIRECTION('ref_axis',(0.,1.,0.));
#9051=DIRECTION('',(0.,1.,0.));
#9052=DIRECTION('',(1.,0.,0.));
#9053=DIRECTION('',(0.,-1.,0.));
#9054=DIRECTION('center_axis',(0.,-0.707106781186547,-0.707106781186548));
#9055=DIRECTION('ref_axis',(0.,0.707106781186548,-0.707106781186547));
#9056=DIRECTION('',(0.,0.707106781186548,-0.707106781186547));
#9057=DIRECTION('',(1.,0.,0.));
#9058=DIRECTION('',(0.,-0.707106781186548,0.707106781186547));
#9059=DIRECTION('center_axis',(0.,-1.,0.));
#9060=DIRECTION('ref_axis',(0.,0.,-1.));
#9061=DIRECTION('',(0.,0.,-1.));
#9062=DIRECTION('',(1.,0.,0.));
#9063=DIRECTION('',(0.,0.,1.));
#9064=DIRECTION('center_axis',(0.,0.,1.));
#9065=DIRECTION('ref_axis',(0.,-1.,0.));
#9066=DIRECTION('',(0.,-1.,0.));
#9067=DIRECTION('',(1.,0.,0.));
#9068=DIRECTION('',(0.,1.,0.));
#9069=DIRECTION('center_axis',(0.,-1.,0.));
#9070=DIRECTION('ref_axis',(0.,0.,-1.));
#9071=DIRECTION('',(0.,0.,-1.));
#9072=DIRECTION('',(-1.,0.,0.));
#9073=DIRECTION('',(0.,0.,1.));
#9074=DIRECTION('center_axis',(1.,0.,0.));
#9075=DIRECTION('ref_axis',(0.,0.,-1.));
#9076=DIRECTION('',(1.,0.,0.));
#9077=DIRECTION('center_axis',(-1.,0.,0.));
#9078=DIRECTION('ref_axis',(0.,0.,-1.));
#9079=DIRECTION('center_axis',(0.,1.,0.));
#9080=DIRECTION('ref_axis',(0.,0.,1.));
#9081=DIRECTION('',(0.,0.,1.));
#9082=DIRECTION('',(1.,0.,0.));
#9083=DIRECTION('',(0.,0.,1.));
#9084=DIRECTION('center_axis',(0.,1.,0.));
#9085=DIRECTION('ref_axis',(0.,0.,1.));
#9086=DIRECTION('',(0.,0.,1.));
#9087=DIRECTION('',(1.,0.,0.));
#9088=DIRECTION('',(0.,0.,1.));
#9089=DIRECTION('center_axis',(0.,0.,-1.));
#9090=DIRECTION('ref_axis',(0.,1.,0.));
#9091=DIRECTION('',(0.,1.,0.));
#9092=DIRECTION('',(0.,1.,0.));
#9093=DIRECTION('center_axis',(0.,0.,-1.));
#9094=DIRECTION('ref_axis',(0.,1.,0.));
#9095=DIRECTION('',(0.,1.,0.));
#9096=DIRECTION('',(1.,0.,0.));
#9097=DIRECTION('',(0.,1.,0.));
#9098=DIRECTION('center_axis',(0.,-1.,0.));
#9099=DIRECTION('ref_axis',(0.,0.,-1.));
#9100=DIRECTION('',(0.,0.,-1.));
#9101=DIRECTION('',(0.,0.,-1.));
#9102=DIRECTION('center_axis',(0.,-1.,0.));
#9103=DIRECTION('ref_axis',(0.,0.,-1.));
#9104=DIRECTION('',(0.,0.,-1.));
#9105=DIRECTION('',(1.,0.,0.));
#9106=DIRECTION('',(0.,0.,-1.));
#9107=DIRECTION('center_axis',(0.,0.,1.));
#9108=DIRECTION('ref_axis',(0.,-1.,0.));
#9109=DIRECTION('',(0.,-1.,0.));
#9110=DIRECTION('',(0.,-1.,0.));
#9111=DIRECTION('center_axis',(0.,0.,1.));
#9112=DIRECTION('ref_axis',(0.,-1.,0.));
#9113=DIRECTION('',(0.,-1.,0.));
#9114=DIRECTION('',(0.,-1.,0.));
#9115=DIRECTION('center_axis',(1.,0.,0.));
#9116=DIRECTION('ref_axis',(0.,0.,-1.));
#9117=DIRECTION('center_axis',(1.,0.,0.));
#9118=DIRECTION('ref_axis',(0.,0.,-1.));
#9119=DIRECTION('axis',(0.,0.,1.));
#9120=DIRECTION('refdir',(1.,0.,0.));
#9121=DIRECTION('center_axis',(0.,0.,1.));
#9122=DIRECTION('ref_axis',(1.,0.,0.));
#9123=DIRECTION('center_axis',(0.,0.,1.));
#9124=DIRECTION('ref_axis',(1.,0.,0.));
#9125=DIRECTION('',(0.,0.,1.));
#9126=DIRECTION('',(0.,0.,1.));
#9127=DIRECTION('center_axis',(0.,0.,-1.));
#9128=DIRECTION('ref_axis',(1.,0.,0.));
#9129=DIRECTION('center_axis',(1.,0.,0.));
#9130=DIRECTION('ref_axis',(0.,0.,-1.));
#9131=DIRECTION('center_axis',(1.,0.,0.));
#9132=DIRECTION('ref_axis',(0.,0.,-1.));
#9133=DIRECTION('',(1.,0.,0.));
#9134=DIRECTION('center_axis',(0.,0.,-1.));
#9135=DIRECTION('ref_axis',(0.,1.,0.));
#9136=DIRECTION('',(0.,1.,0.));
#9137=DIRECTION('',(1.,0.,0.));
#9138=DIRECTION('',(0.,-1.,0.));
#9139=DIRECTION('',(1.,0.,0.));
#9140=DIRECTION('center_axis',(0.,1.,-8.88178419700125E-16));
#9141=DIRECTION('ref_axis',(0.,8.88178419700125E-16,1.));
#9142=DIRECTION('',(0.,8.88178419700125E-16,1.));
#9143=DIRECTION('',(1.,0.,0.));
#9144=DIRECTION('',(0.,-8.88178419700125E-16,-1.));
#9145=DIRECTION('center_axis',(0.,-7.40148683083439E-16,-1.));
#9146=DIRECTION('ref_axis',(0.,1.,-7.40148683083439E-16));
#9147=DIRECTION('',(0.,1.,-7.40148683083439E-16));
#9148=DIRECTION('',(1.,0.,0.));
#9149=DIRECTION('',(0.,-1.,7.40148683083439E-16));
#9150=DIRECTION('center_axis',(0.,-0.707106781186547,-0.707106781186548));
#9151=DIRECTION('ref_axis',(0.,0.707106781186548,-0.707106781186547));
#9152=DIRECTION('',(0.,0.707106781186548,-0.707106781186547));
#9153=DIRECTION('',(1.,0.,0.));
#9154=DIRECTION('',(0.,-0.707106781186548,0.707106781186547));
#9155=DIRECTION('center_axis',(0.,-1.,2.77555756156289E-16));
#9156=DIRECTION('ref_axis',(0.,-2.77555756156289E-16,-1.));
#9157=DIRECTION('',(0.,-2.77555756156289E-16,-1.));
#9158=DIRECTION('',(1.,0.,0.));
#9159=DIRECTION('',(0.,2.77555756156289E-16,1.));
#9160=DIRECTION('center_axis',(0.,-0.707106781186547,0.707106781186548));
#9161=DIRECTION('ref_axis',(0.,-0.707106781186548,-0.707106781186547));
#9162=DIRECTION('',(0.,-0.707106781186548,-0.707106781186547));
#9163=DIRECTION('',(1.,0.,0.));
#9164=DIRECTION('',(0.,0.707106781186548,0.707106781186547));
#9165=DIRECTION('center_axis',(0.,7.40148683083438E-16,1.));
#9166=DIRECTION('ref_axis',(0.,-1.,7.40148683083438E-16));
#9167=DIRECTION('',(0.,-1.,7.40148683083438E-16));
#9168=DIRECTION('',(1.,0.,0.));
#9169=DIRECTION('',(0.,1.,-7.40148683083438E-16));
#9170=DIRECTION('center_axis',(0.,1.,-4.44089209850063E-16));
#9171=DIRECTION('ref_axis',(0.,4.44089209850063E-16,1.));
#9172=DIRECTION('',(0.,4.44089209850063E-16,1.));
#9173=DIRECTION('',(1.,0.,0.));
#9174=DIRECTION('',(0.,-4.44089209850063E-16,-1.));
#9175=DIRECTION('center_axis',(0.,2.41352831440251E-16,1.));
#9176=DIRECTION('ref_axis',(0.,-1.,2.41352831440251E-16));
#9177=DIRECTION('',(0.,-1.,2.41352831440251E-16));
#9178=DIRECTION('',(-1.,0.,0.));
#9179=DIRECTION('',(0.,1.,-2.41352831440251E-16));
#9180=DIRECTION('center_axis',(0.,-1.,2.41352831440251E-16));
#9181=DIRECTION('ref_axis',(0.,-2.41352831440251E-16,-1.));
#9182=DIRECTION('',(0.,-2.41352831440251E-16,-1.));
#9183=DIRECTION('',(1.,0.,0.));
#9184=DIRECTION('',(0.,2.41352831440251E-16,1.));
#9185=DIRECTION('',(1.,0.,0.));
#9186=DIRECTION('center_axis',(0.,0.,-1.));
#9187=DIRECTION('ref_axis',(0.,1.,0.));
#9188=DIRECTION('',(0.,1.,0.));
#9189=DIRECTION('',(1.,0.,0.));
#9190=DIRECTION('',(0.,-1.,0.));
#9191=DIRECTION('center_axis',(0.,-1.,0.));
#9192=DIRECTION('ref_axis',(0.,0.,-1.));
#9193=DIRECTION('',(0.,0.,-1.));
#9194=DIRECTION('',(1.,0.,0.));
#9195=DIRECTION('',(0.,0.,1.));
#9196=DIRECTION('center_axis',(0.,-0.707106781186547,0.707106781186548));
#9197=DIRECTION('ref_axis',(0.,-0.707106781186548,-0.707106781186547));
#9198=DIRECTION('',(0.,-0.707106781186548,-0.707106781186547));
#9199=DIRECTION('',(1.,0.,0.));
#9200=DIRECTION('',(0.,0.707106781186548,0.707106781186547));
#9201=DIRECTION('center_axis',(0.,0.,1.));
#9202=DIRECTION('ref_axis',(0.,-1.,0.));
#9203=DIRECTION('',(0.,-1.,0.));
#9204=DIRECTION('',(1.,0.,0.));
#9205=DIRECTION('',(0.,1.,0.));
#9206=DIRECTION('center_axis',(0.,0.707106781186548,0.707106781186547));
#9207=DIRECTION('ref_axis',(0.,-0.707106781186547,0.707106781186548));
#9208=DIRECTION('',(0.,-0.707106781186547,0.707106781186548));
#9209=DIRECTION('',(1.,0.,0.));
#9210=DIRECTION('',(0.,0.707106781186547,-0.707106781186548));
#9211=DIRECTION('center_axis',(0.,1.,0.));
#9212=DIRECTION('ref_axis',(0.,0.,1.));
#9213=DIRECTION('',(0.,0.,1.));
#9214=DIRECTION('',(1.,0.,0.));
#9215=DIRECTION('',(0.,0.,-1.));
#9216=DIRECTION('center_axis',(0.,0.,-1.));
#9217=DIRECTION('ref_axis',(0.,1.,0.));
#9218=DIRECTION('',(0.,1.,0.));
#9219=DIRECTION('',(1.,0.,0.));
#9220=DIRECTION('',(0.,-1.,0.));
#9221=DIRECTION('center_axis',(0.,1.,-2.41352831440251E-16));
#9222=DIRECTION('ref_axis',(0.,2.41352831440251E-16,1.));
#9223=DIRECTION('',(0.,2.41352831440251E-16,1.));
#9224=DIRECTION('',(-1.,0.,0.));
#9225=DIRECTION('',(0.,-2.41352831440251E-16,-1.));
#9226=DIRECTION('center_axis',(0.,0.,1.));
#9227=DIRECTION('ref_axis',(0.,-1.,0.));
#9228=DIRECTION('',(0.,-1.,0.));
#9229=DIRECTION('',(1.,0.,0.));
#9230=DIRECTION('',(0.,1.,0.));
#9231=DIRECTION('',(1.,0.,0.));
#9232=DIRECTION('center_axis',(0.,-1.,0.));
#9233=DIRECTION('ref_axis',(0.,0.,-1.));
#9234=DIRECTION('',(0.,0.,-1.));
#9235=DIRECTION('',(1.,0.,0.));
#9236=DIRECTION('',(0.,0.,1.));
#9237=DIRECTION('center_axis',(0.,0.,1.));
#9238=DIRECTION('ref_axis',(0.,-1.,0.));
#9239=DIRECTION('',(0.,-1.,0.));
#9240=DIRECTION('',(1.,0.,0.));
#9241=DIRECTION('',(0.,1.,0.));
#9242=DIRECTION('center_axis',(0.,0.707106781186548,0.707106781186548));
#9243=DIRECTION('ref_axis',(0.,-0.707106781186548,0.707106781186548));
#9244=DIRECTION('',(0.,-0.707106781186548,0.707106781186548));
#9245=DIRECTION('',(1.,0.,0.));
#9246=DIRECTION('',(0.,0.707106781186548,-0.707106781186548));
#9247=DIRECTION('center_axis',(0.,1.,0.));
#9248=DIRECTION('ref_axis',(0.,0.,1.));
#9249=DIRECTION('',(0.,0.,1.));
#9250=DIRECTION('',(1.,0.,0.));
#9251=DIRECTION('',(0.,0.,-1.));
#9252=DIRECTION('center_axis',(0.,0.707106781186548,-0.707106781186547));
#9253=DIRECTION('ref_axis',(0.,0.707106781186547,0.707106781186548));
#9254=DIRECTION('',(0.,0.707106781186547,0.707106781186548));
#9255=DIRECTION('',(1.,0.,0.));
#9256=DIRECTION('',(0.,-0.707106781186547,-0.707106781186548));
#9257=DIRECTION('center_axis',(0.,-7.40148683083438E-16,-1.));
#9258=DIRECTION('ref_axis',(0.,1.,-7.40148683083438E-16));
#9259=DIRECTION('',(0.,1.,-7.40148683083438E-16));
#9260=DIRECTION('',(1.,0.,0.));
#9261=DIRECTION('',(0.,-1.,7.40148683083438E-16));
#9262=DIRECTION('center_axis',(0.,-1.,0.));
#9263=DIRECTION('ref_axis',(0.,0.,-1.));
#9264=DIRECTION('',(0.,0.,-1.));
#9265=DIRECTION('',(1.,0.,0.));
#9266=DIRECTION('',(0.,0.,1.));
#9267=DIRECTION('center_axis',(0.,0.,-1.));
#9268=DIRECTION('ref_axis',(0.,1.,0.));
#9269=DIRECTION('',(0.,1.,0.));
#9270=DIRECTION('',(-1.,0.,0.));
#9271=DIRECTION('',(0.,-1.,0.));
#9272=DIRECTION('center_axis',(0.,1.,0.));
#9273=DIRECTION('ref_axis',(0.,0.,1.));
#9274=DIRECTION('',(0.,0.,1.));
#9275=DIRECTION('',(1.,0.,0.));
#9276=DIRECTION('',(0.,0.,-1.));
#9277=DIRECTION('',(1.,0.,0.));
#9278=DIRECTION('center_axis',(0.,0.,1.));
#9279=DIRECTION('ref_axis',(0.,-1.,0.));
#9280=DIRECTION('',(0.,-1.,0.));
#9281=DIRECTION('',(1.,0.,0.));
#9282=DIRECTION('',(0.,1.,0.));
#9283=DIRECTION('center_axis',(0.,1.,0.));
#9284=DIRECTION('ref_axis',(0.,0.,1.));
#9285=DIRECTION('',(0.,0.,1.));
#9286=DIRECTION('',(1.,0.,0.));
#9287=DIRECTION('',(0.,0.,-1.));
#9288=DIRECTION('center_axis',(0.,0.707106781186547,-0.707106781186548));
#9289=DIRECTION('ref_axis',(0.,0.707106781186548,0.707106781186547));
#9290=DIRECTION('',(0.,0.707106781186548,0.707106781186547));
#9291=DIRECTION('',(1.,0.,0.));
#9292=DIRECTION('',(0.,-0.707106781186548,-0.707106781186547));
#9293=DIRECTION('center_axis',(0.,0.,-1.));
#9294=DIRECTION('ref_axis',(0.,1.,0.));
#9295=DIRECTION('',(0.,1.,0.));
#9296=DIRECTION('',(1.,0.,0.));
#9297=DIRECTION('',(0.,-1.,0.));
#9298=DIRECTION('center_axis',(0.,-0.707106781186547,-0.707106781186548));
#9299=DIRECTION('ref_axis',(0.,0.707106781186548,-0.707106781186547));
#9300=DIRECTION('',(0.,0.707106781186548,-0.707106781186547));
#9301=DIRECTION('',(1.,0.,0.));
#9302=DIRECTION('',(0.,-0.707106781186548,0.707106781186547));
#9303=DIRECTION('center_axis',(0.,-1.,0.));
#9304=DIRECTION('ref_axis',(0.,0.,-1.));
#9305=DIRECTION('',(0.,0.,-1.));
#9306=DIRECTION('',(1.,0.,0.));
#9307=DIRECTION('',(0.,0.,1.));
#9308=DIRECTION('center_axis',(0.,0.,1.));
#9309=DIRECTION('ref_axis',(0.,-1.,0.));
#9310=DIRECTION('',(0.,-1.,0.));
#9311=DIRECTION('',(1.,0.,0.));
#9312=DIRECTION('',(0.,1.,0.));
#9313=DIRECTION('center_axis',(0.,-1.,0.));
#9314=DIRECTION('ref_axis',(0.,0.,-1.));
#9315=DIRECTION('',(0.,0.,-1.));
#9316=DIRECTION('',(-1.,0.,0.));
#9317=DIRECTION('',(0.,0.,1.));
#9318=DIRECTION('center_axis',(1.,0.,0.));
#9319=DIRECTION('ref_axis',(0.,0.,-1.));
#9320=DIRECTION('',(1.,0.,0.));
#9321=DIRECTION('center_axis',(-1.,0.,0.));
#9322=DIRECTION('ref_axis',(0.,0.,-1.));
#9323=DIRECTION('center_axis',(0.,1.,0.));
#9324=DIRECTION('ref_axis',(0.,0.,1.));
#9325=DIRECTION('',(0.,0.,1.));
#9326=DIRECTION('',(1.,0.,0.));
#9327=DIRECTION('',(0.,0.,1.));
#9328=DIRECTION('center_axis',(0.,1.,0.));
#9329=DIRECTION('ref_axis',(0.,0.,1.));
#9330=DIRECTION('',(0.,0.,1.));
#9331=DIRECTION('',(1.,0.,0.));
#9332=DIRECTION('',(0.,0.,1.));
#9333=DIRECTION('center_axis',(0.,0.,-1.));
#9334=DIRECTION('ref_axis',(0.,1.,0.));
#9335=DIRECTION('',(0.,1.,0.));
#9336=DIRECTION('',(0.,1.,0.));
#9337=DIRECTION('center_axis',(0.,0.,-1.));
#9338=DIRECTION('ref_axis',(0.,1.,0.));
#9339=DIRECTION('',(0.,1.,0.));
#9340=DIRECTION('',(1.,0.,0.));
#9341=DIRECTION('',(0.,1.,0.));
#9342=DIRECTION('center_axis',(0.,-1.,0.));
#9343=DIRECTION('ref_axis',(0.,0.,-1.));
#9344=DIRECTION('',(0.,0.,-1.));
#9345=DIRECTION('',(0.,0.,-1.));
#9346=DIRECTION('center_axis',(0.,-1.,0.));
#9347=DIRECTION('ref_axis',(0.,0.,-1.));
#9348=DIRECTION('',(0.,0.,-1.));
#9349=DIRECTION('',(1.,0.,0.));
#9350=DIRECTION('',(0.,0.,-1.));
#9351=DIRECTION('center_axis',(0.,0.,1.));
#9352=DIRECTION('ref_axis',(0.,-1.,0.));
#9353=DIRECTION('',(0.,-1.,0.));
#9354=DIRECTION('',(0.,-1.,0.));
#9355=DIRECTION('center_axis',(0.,0.,1.));
#9356=DIRECTION('ref_axis',(0.,-1.,0.));
#9357=DIRECTION('',(0.,-1.,0.));
#9358=DIRECTION('',(0.,-1.,0.));
#9359=DIRECTION('center_axis',(1.,0.,0.));
#9360=DIRECTION('ref_axis',(0.,0.,-1.));
#9361=DIRECTION('center_axis',(1.,0.,0.));
#9362=DIRECTION('ref_axis',(0.,0.,-1.));
#9363=DIRECTION('axis',(0.,0.,1.));
#9364=DIRECTION('refdir',(1.,0.,0.));
#9365=DIRECTION('center_axis',(0.,0.,-1.));
#9366=DIRECTION('ref_axis',(0.,1.,0.));
#9367=DIRECTION('',(0.,1.,0.));
#9368=DIRECTION('',(1.,0.,0.));
#9369=DIRECTION('',(0.,-1.,0.));
#9370=DIRECTION('',(1.,0.,0.));
#9371=DIRECTION('center_axis',(0.,1.,-8.88178419700125E-16));
#9372=DIRECTION('ref_axis',(0.,8.88178419700125E-16,1.));
#9373=DIRECTION('',(0.,8.88178419700125E-16,1.));
#9374=DIRECTION('',(1.,0.,0.));
#9375=DIRECTION('',(0.,-8.88178419700125E-16,-1.));
#9376=DIRECTION('center_axis',(0.,-7.40148683083439E-16,-1.));
#9377=DIRECTION('ref_axis',(0.,1.,-7.40148683083439E-16));
#9378=DIRECTION('',(0.,1.,-7.40148683083439E-16));
#9379=DIRECTION('',(1.,0.,0.));
#9380=DIRECTION('',(0.,-1.,7.40148683083439E-16));
#9381=DIRECTION('center_axis',(0.,-0.707106781186547,-0.707106781186548));
#9382=DIRECTION('ref_axis',(0.,0.707106781186548,-0.707106781186547));
#9383=DIRECTION('',(0.,0.707106781186548,-0.707106781186547));
#9384=DIRECTION('',(1.,0.,0.));
#9385=DIRECTION('',(0.,-0.707106781186548,0.707106781186547));
#9386=DIRECTION('center_axis',(0.,-1.,2.77555756156289E-16));
#9387=DIRECTION('ref_axis',(0.,-2.77555756156289E-16,-1.));
#9388=DIRECTION('',(0.,-2.77555756156289E-16,-1.));
#9389=DIRECTION('',(1.,0.,0.));
#9390=DIRECTION('',(0.,2.77555756156289E-16,1.));
#9391=DIRECTION('center_axis',(0.,-0.707106781186547,0.707106781186548));
#9392=DIRECTION('ref_axis',(0.,-0.707106781186548,-0.707106781186547));
#9393=DIRECTION('',(0.,-0.707106781186548,-0.707106781186547));
#9394=DIRECTION('',(1.,0.,0.));
#9395=DIRECTION('',(0.,0.707106781186548,0.707106781186547));
#9396=DIRECTION('center_axis',(0.,7.40148683083438E-16,1.));
#9397=DIRECTION('ref_axis',(0.,-1.,7.40148683083438E-16));
#9398=DIRECTION('',(0.,-1.,7.40148683083438E-16));
#9399=DIRECTION('',(1.,0.,0.));
#9400=DIRECTION('',(0.,1.,-7.40148683083438E-16));
#9401=DIRECTION('center_axis',(0.,1.,-4.44089209850063E-16));
#9402=DIRECTION('ref_axis',(0.,4.44089209850063E-16,1.));
#9403=DIRECTION('',(0.,4.44089209850063E-16,1.));
#9404=DIRECTION('',(1.,0.,0.));
#9405=DIRECTION('',(0.,-4.44089209850063E-16,-1.));
#9406=DIRECTION('center_axis',(0.,2.41352831440251E-16,1.));
#9407=DIRECTION('ref_axis',(0.,-1.,2.41352831440251E-16));
#9408=DIRECTION('',(0.,-1.,2.41352831440251E-16));
#9409=DIRECTION('',(-1.,0.,0.));
#9410=DIRECTION('',(0.,1.,-2.41352831440251E-16));
#9411=DIRECTION('center_axis',(0.,-1.,2.41352831440251E-16));
#9412=DIRECTION('ref_axis',(0.,-2.41352831440251E-16,-1.));
#9413=DIRECTION('',(0.,-2.41352831440251E-16,-1.));
#9414=DIRECTION('',(1.,0.,0.));
#9415=DIRECTION('',(0.,2.41352831440251E-16,1.));
#9416=DIRECTION('',(1.,0.,0.));
#9417=DIRECTION('center_axis',(0.,0.,-1.));
#9418=DIRECTION('ref_axis',(0.,1.,0.));
#9419=DIRECTION('',(0.,1.,0.));
#9420=DIRECTION('',(1.,0.,0.));
#9421=DIRECTION('',(0.,-1.,0.));
#9422=DIRECTION('center_axis',(0.,-1.,0.));
#9423=DIRECTION('ref_axis',(0.,0.,-1.));
#9424=DIRECTION('',(0.,0.,-1.));
#9425=DIRECTION('',(1.,0.,0.));
#9426=DIRECTION('',(0.,0.,1.));
#9427=DIRECTION('center_axis',(0.,-0.707106781186547,0.707106781186548));
#9428=DIRECTION('ref_axis',(0.,-0.707106781186548,-0.707106781186547));
#9429=DIRECTION('',(0.,-0.707106781186548,-0.707106781186547));
#9430=DIRECTION('',(1.,0.,0.));
#9431=DIRECTION('',(0.,0.707106781186548,0.707106781186547));
#9432=DIRECTION('center_axis',(0.,0.,1.));
#9433=DIRECTION('ref_axis',(0.,-1.,0.));
#9434=DIRECTION('',(0.,-1.,0.));
#9435=DIRECTION('',(1.,0.,0.));
#9436=DIRECTION('',(0.,1.,0.));
#9437=DIRECTION('center_axis',(0.,0.707106781186548,0.707106781186547));
#9438=DIRECTION('ref_axis',(0.,-0.707106781186547,0.707106781186548));
#9439=DIRECTION('',(0.,-0.707106781186547,0.707106781186548));
#9440=DIRECTION('',(1.,0.,0.));
#9441=DIRECTION('',(0.,0.707106781186547,-0.707106781186548));
#9442=DIRECTION('center_axis',(0.,1.,0.));
#9443=DIRECTION('ref_axis',(0.,0.,1.));
#9444=DIRECTION('',(0.,0.,1.));
#9445=DIRECTION('',(1.,0.,0.));
#9446=DIRECTION('',(0.,0.,-1.));
#9447=DIRECTION('center_axis',(0.,0.,-1.));
#9448=DIRECTION('ref_axis',(0.,1.,0.));
#9449=DIRECTION('',(0.,1.,0.));
#9450=DIRECTION('',(1.,0.,0.));
#9451=DIRECTION('',(0.,-1.,0.));
#9452=DIRECTION('center_axis',(0.,1.,-2.41352831440251E-16));
#9453=DIRECTION('ref_axis',(0.,2.41352831440251E-16,1.));
#9454=DIRECTION('',(0.,2.41352831440251E-16,1.));
#9455=DIRECTION('',(-1.,0.,0.));
#9456=DIRECTION('',(0.,-2.41352831440251E-16,-1.));
#9457=DIRECTION('center_axis',(0.,0.,1.));
#9458=DIRECTION('ref_axis',(0.,-1.,0.));
#9459=DIRECTION('',(0.,-1.,0.));
#9460=DIRECTION('',(1.,0.,0.));
#9461=DIRECTION('',(0.,1.,0.));
#9462=DIRECTION('',(1.,0.,0.));
#9463=DIRECTION('center_axis',(0.,-1.,0.));
#9464=DIRECTION('ref_axis',(0.,0.,-1.));
#9465=DIRECTION('',(0.,0.,-1.));
#9466=DIRECTION('',(1.,0.,0.));
#9467=DIRECTION('',(0.,0.,1.));
#9468=DIRECTION('center_axis',(0.,0.,1.));
#9469=DIRECTION('ref_axis',(0.,-1.,0.));
#9470=DIRECTION('',(0.,-1.,0.));
#9471=DIRECTION('',(1.,0.,0.));
#9472=DIRECTION('',(0.,1.,0.));
#9473=DIRECTION('center_axis',(0.,0.707106781186548,0.707106781186548));
#9474=DIRECTION('ref_axis',(0.,-0.707106781186548,0.707106781186548));
#9475=DIRECTION('',(0.,-0.707106781186548,0.707106781186548));
#9476=DIRECTION('',(1.,0.,0.));
#9477=DIRECTION('',(0.,0.707106781186548,-0.707106781186548));
#9478=DIRECTION('center_axis',(0.,1.,0.));
#9479=DIRECTION('ref_axis',(0.,0.,1.));
#9480=DIRECTION('',(0.,0.,1.));
#9481=DIRECTION('',(1.,0.,0.));
#9482=DIRECTION('',(0.,0.,-1.));
#9483=DIRECTION('center_axis',(0.,0.707106781186548,-0.707106781186547));
#9484=DIRECTION('ref_axis',(0.,0.707106781186547,0.707106781186548));
#9485=DIRECTION('',(0.,0.707106781186547,0.707106781186548));
#9486=DIRECTION('',(1.,0.,0.));
#9487=DIRECTION('',(0.,-0.707106781186547,-0.707106781186548));
#9488=DIRECTION('center_axis',(0.,-7.40148683083438E-16,-1.));
#9489=DIRECTION('ref_axis',(0.,1.,-7.40148683083438E-16));
#9490=DIRECTION('',(0.,1.,-7.40148683083438E-16));
#9491=DIRECTION('',(1.,0.,0.));
#9492=DIRECTION('',(0.,-1.,7.40148683083438E-16));
#9493=DIRECTION('center_axis',(0.,-1.,0.));
#9494=DIRECTION('ref_axis',(0.,0.,-1.));
#9495=DIRECTION('',(0.,0.,-1.));
#9496=DIRECTION('',(1.,0.,0.));
#9497=DIRECTION('',(0.,0.,1.));
#9498=DIRECTION('center_axis',(0.,0.,-1.));
#9499=DIRECTION('ref_axis',(0.,1.,0.));
#9500=DIRECTION('',(0.,1.,0.));
#9501=DIRECTION('',(-1.,0.,0.));
#9502=DIRECTION('',(0.,-1.,0.));
#9503=DIRECTION('center_axis',(0.,1.,0.));
#9504=DIRECTION('ref_axis',(0.,0.,1.));
#9505=DIRECTION('',(0.,0.,1.));
#9506=DIRECTION('',(1.,0.,0.));
#9507=DIRECTION('',(0.,0.,-1.));
#9508=DIRECTION('',(1.,0.,0.));
#9509=DIRECTION('center_axis',(0.,0.,1.));
#9510=DIRECTION('ref_axis',(0.,-1.,0.));
#9511=DIRECTION('',(0.,-1.,0.));
#9512=DIRECTION('',(1.,0.,0.));
#9513=DIRECTION('',(0.,1.,0.));
#9514=DIRECTION('center_axis',(0.,1.,0.));
#9515=DIRECTION('ref_axis',(0.,0.,1.));
#9516=DIRECTION('',(0.,0.,1.));
#9517=DIRECTION('',(1.,0.,0.));
#9518=DIRECTION('',(0.,0.,-1.));
#9519=DIRECTION('center_axis',(0.,0.707106781186547,-0.707106781186548));
#9520=DIRECTION('ref_axis',(0.,0.707106781186548,0.707106781186547));
#9521=DIRECTION('',(0.,0.707106781186548,0.707106781186547));
#9522=DIRECTION('',(1.,0.,0.));
#9523=DIRECTION('',(0.,-0.707106781186548,-0.707106781186547));
#9524=DIRECTION('center_axis',(0.,0.,-1.));
#9525=DIRECTION('ref_axis',(0.,1.,0.));
#9526=DIRECTION('',(0.,1.,0.));
#9527=DIRECTION('',(1.,0.,0.));
#9528=DIRECTION('',(0.,-1.,0.));
#9529=DIRECTION('center_axis',(0.,-0.707106781186547,-0.707106781186548));
#9530=DIRECTION('ref_axis',(0.,0.707106781186548,-0.707106781186547));
#9531=DIRECTION('',(0.,0.707106781186548,-0.707106781186547));
#9532=DIRECTION('',(1.,0.,0.));
#9533=DIRECTION('',(0.,-0.707106781186548,0.707106781186547));
#9534=DIRECTION('center_axis',(0.,-1.,0.));
#9535=DIRECTION('ref_axis',(0.,0.,-1.));
#9536=DIRECTION('',(0.,0.,-1.));
#9537=DIRECTION('',(1.,0.,0.));
#9538=DIRECTION('',(0.,0.,1.));
#9539=DIRECTION('center_axis',(0.,0.,1.));
#9540=DIRECTION('ref_axis',(0.,-1.,0.));
#9541=DIRECTION('',(0.,-1.,0.));
#9542=DIRECTION('',(1.,0.,0.));
#9543=DIRECTION('',(0.,1.,0.));
#9544=DIRECTION('center_axis',(0.,-1.,0.));
#9545=DIRECTION('ref_axis',(0.,0.,-1.));
#9546=DIRECTION('',(0.,0.,-1.));
#9547=DIRECTION('',(-1.,0.,0.));
#9548=DIRECTION('',(0.,0.,1.));
#9549=DIRECTION('center_axis',(1.,0.,0.));
#9550=DIRECTION('ref_axis',(0.,0.,-1.));
#9551=DIRECTION('center_axis',(1.,0.,0.));
#9552=DIRECTION('ref_axis',(0.,0.,-1.));
#9553=DIRECTION('',(1.,0.,0.));
#9554=DIRECTION('center_axis',(-1.,0.,0.));
#9555=DIRECTION('ref_axis',(0.,0.,-1.));
#9556=DIRECTION('center_axis',(0.,1.,0.));
#9557=DIRECTION('ref_axis',(0.,0.,1.));
#9558=DIRECTION('',(0.,0.,1.));
#9559=DIRECTION('',(1.,0.,0.));
#9560=DIRECTION('',(0.,0.,1.));
#9561=DIRECTION('center_axis',(0.,1.,0.));
#9562=DIRECTION('ref_axis',(0.,0.,1.));
#9563=DIRECTION('',(0.,0.,1.));
#9564=DIRECTION('',(1.,0.,0.));
#9565=DIRECTION('',(0.,0.,1.));
#9566=DIRECTION('center_axis',(0.,0.,-1.));
#9567=DIRECTION('ref_axis',(0.,1.,0.));
#9568=DIRECTION('',(0.,1.,0.));
#9569=DIRECTION('',(0.,1.,0.));
#9570=DIRECTION('center_axis',(0.,0.,-1.));
#9571=DIRECTION('ref_axis',(0.,1.,0.));
#9572=DIRECTION('',(0.,1.,0.));
#9573=DIRECTION('',(1.,0.,0.));
#9574=DIRECTION('',(0.,1.,0.));
#9575=DIRECTION('center_axis',(0.,-1.,0.));
#9576=DIRECTION('ref_axis',(0.,0.,-1.));
#9577=DIRECTION('',(0.,0.,-1.));
#9578=DIRECTION('',(0.,0.,-1.));
#9579=DIRECTION('center_axis',(0.,-1.,0.));
#9580=DIRECTION('ref_axis',(0.,0.,-1.));
#9581=DIRECTION('',(0.,0.,-1.));
#9582=DIRECTION('',(1.,0.,0.));
#9583=DIRECTION('',(0.,0.,-1.));
#9584=DIRECTION('center_axis',(0.,0.,1.));
#9585=DIRECTION('ref_axis',(0.,-1.,0.));
#9586=DIRECTION('',(0.,-1.,0.));
#9587=DIRECTION('',(0.,-1.,0.));
#9588=DIRECTION('center_axis',(0.,0.,1.));
#9589=DIRECTION('ref_axis',(0.,-1.,0.));
#9590=DIRECTION('',(0.,-1.,0.));
#9591=DIRECTION('',(0.,-1.,0.));
#9592=DIRECTION('center_axis',(1.,0.,0.));
#9593=DIRECTION('ref_axis',(0.,0.,-1.));
#9594=DIRECTION('center_axis',(1.,0.,0.));
#9595=DIRECTION('ref_axis',(0.,0.,-1.));
#9596=DIRECTION('axis',(0.,0.,1.));
#9597=DIRECTION('refdir',(1.,0.,0.));
#9598=DIRECTION('center_axis',(0.866025403784439,0.,-0.5));
#9599=DIRECTION('ref_axis',(0.5,0.,0.866025403784439));
#9600=DIRECTION('',(-0.5,0.,-0.866025403784439));
#9601=DIRECTION('',(0.,-1.,0.));
#9602=DIRECTION('',(0.5,0.,0.866025403784439));
#9603=DIRECTION('',(0.,-1.,0.));
#9604=DIRECTION('center_axis',(1.20185167898973E-16,0.,-1.));
#9605=DIRECTION('ref_axis',(1.,0.,1.20185167898973E-16));
#9606=DIRECTION('',(-1.,0.,-1.20185167898973E-16));
#9607=DIRECTION('',(0.,-1.,0.));
#9608=DIRECTION('',(1.,0.,1.20185167898973E-16));
#9609=DIRECTION('center_axis',(-0.866025403784439,0.,-0.5));
#9610=DIRECTION('ref_axis',(0.5,0.,-0.866025403784439));
#9611=DIRECTION('',(-0.5,0.,0.866025403784439));
#9612=DIRECTION('',(0.,-1.,0.));
#9613=DIRECTION('',(0.5,0.,-0.866025403784439));
#9614=DIRECTION('center_axis',(-0.866025403784439,0.,0.5));
#9615=DIRECTION('ref_axis',(-0.5,0.,-0.866025403784439));
#9616=DIRECTION('',(0.5,0.,0.866025403784439));
#9617=DIRECTION('',(0.,-1.,0.));
#9618=DIRECTION('',(-0.5,0.,-0.866025403784439));
#9619=DIRECTION('center_axis',(-2.40370335797945E-16,0.,1.));
#9620=DIRECTION('ref_axis',(-1.,0.,-2.40370335797945E-16));
#9621=DIRECTION('',(1.,0.,2.40370335797945E-16));
#9622=DIRECTION('',(0.,-1.,0.));
#9623=DIRECTION('',(-1.,0.,-2.40370335797945E-16));
#9624=DIRECTION('center_axis',(0.866025403784439,0.,0.5));
#9625=DIRECTION('ref_axis',(-0.5,0.,0.866025403784439));
#9626=DIRECTION('',(0.5,0.,-0.866025403784439));
#9627=DIRECTION('',(-0.5,0.,0.866025403784439));
#9628=DIRECTION('center_axis',(0.,1.,0.));
#9629=DIRECTION('ref_axis',(1.,0.,0.));
#9630=DIRECTION('center_axis',(0.,-1.,0.));
#9631=DIRECTION('ref_axis',(0.,0.,-1.));
#9632=DIRECTION('center_axis',(0.,1.,0.));
#9633=DIRECTION('ref_axis',(1.,0.,0.));
#9634=DIRECTION('center_axis',(0.,1.,0.));
#9635=DIRECTION('ref_axis',(1.,0.,0.));
#9636=DIRECTION('center_axis',(0.,1.,0.));
#9637=DIRECTION('ref_axis',(1.,0.,0.));
#9638=DIRECTION('center_axis',(0.,1.,0.));
#9639=DIRECTION('ref_axis',(1.,0.,0.));
#9640=DIRECTION('',(0.,-1.,0.));
#9641=DIRECTION('center_axis',(0.,1.,0.));
#9642=DIRECTION('ref_axis',(1.,0.,0.));
#9643=DIRECTION('center_axis',(0.,1.,0.));
#9644=DIRECTION('ref_axis',(1.,0.,0.));
#9645=DIRECTION('center_axis',(0.,1.,0.));
#9646=DIRECTION('ref_axis',(0.,0.,1.));
#9647=DIRECTION('center_axis',(0.,-1.,0.));
#9648=DIRECTION('ref_axis',(1.,0.,0.));
#9649=DIRECTION('center_axis',(0.,-1.,0.));
#9650=DIRECTION('ref_axis',(1.,0.,0.));
#9651=DIRECTION('center_axis',(0.,-1.,0.));
#9652=DIRECTION('ref_axis',(1.,0.,0.));
#9653=DIRECTION('',(0.707106781186548,0.707106781186547,8.65956056235493E-17));
#9654=DIRECTION('center_axis',(0.,-1.,0.));
#9655=DIRECTION('ref_axis',(1.,0.,0.));
#9656=DIRECTION('center_axis',(0.,-1.,0.));
#9657=DIRECTION('ref_axis',(1.,0.,0.));
#9658=DIRECTION('',(0.,1.,0.));
#9659=DIRECTION('center_axis',(0.,1.,0.));
#9660=DIRECTION('ref_axis',(1.,0.,0.));
#9661=DIRECTION('center_axis',(0.,-1.,0.));
#9662=DIRECTION('ref_axis',(1.,0.,0.));
#9663=DIRECTION('',(-0.707106781186547,0.707106781186548,-8.65956056235493E-17));
#9664=DIRECTION('center_axis',(0.,-1.,0.));
#9665=DIRECTION('ref_axis',(0.,0.,-1.));
#9666=DIRECTION('center_axis',(0.,-1.,0.));
#9667=DIRECTION('ref_axis',(1.,0.,0.));
#9668=DIRECTION('center_axis',(0.,1.,0.));
#9669=DIRECTION('ref_axis',(1.,0.,0.));
#9670=DIRECTION('center_axis',(0.,1.,0.));
#9671=DIRECTION('ref_axis',(1.,0.,0.));
#9672=DIRECTION('',(-0.447213595499958,0.894427190999916,-5.47678698264203E-17));
#9673=DIRECTION('center_axis',(0.,-1.,0.));
#9674=DIRECTION('ref_axis',(1.,0.,0.));
#9675=DIRECTION('',(0.,1.,0.));
#9676=DIRECTION('axis',(0.,0.,1.));
#9677=DIRECTION('refdir',(1.,0.,0.));
#9678=DIRECTION('center_axis',(0.,1.,0.));
#9679=DIRECTION('ref_axis',(0.,0.,1.));
#9680=DIRECTION('center_axis',(0.,-1.,0.));
#9681=DIRECTION('ref_axis',(1.,0.,0.));
#9682=DIRECTION('center_axis',(0.,-1.,0.));
#9683=DIRECTION('ref_axis',(1.,0.,0.));
#9684=DIRECTION('center_axis',(0.,-1.,0.));
#9685=DIRECTION('ref_axis',(1.,0.,0.));
#9686=DIRECTION('',(0.707106781186548,0.707106781186547,8.65956056235493E-17));
#9687=DIRECTION('center_axis',(0.,-1.,0.));
#9688=DIRECTION('ref_axis',(1.,0.,0.));
#9689=DIRECTION('center_axis',(0.,-1.,0.));
#9690=DIRECTION('ref_axis',(1.,0.,0.));
#9691=DIRECTION('',(0.,1.,0.));
#9692=DIRECTION('center_axis',(0.,1.,0.));
#9693=DIRECTION('ref_axis',(1.,0.,0.));
#9694=DIRECTION('center_axis',(0.,-1.,0.));
#9695=DIRECTION('ref_axis',(1.,0.,0.));
#9696=DIRECTION('',(-0.707106781186547,0.707106781186548,-8.65956056235493E-17));
#9697=DIRECTION('center_axis',(0.,-1.,0.));
#9698=DIRECTION('ref_axis',(0.,0.,-1.));
#9699=DIRECTION('center_axis',(0.,-1.,0.));
#9700=DIRECTION('ref_axis',(1.,0.,0.));
#9701=DIRECTION('center_axis',(0.,1.,0.));
#9702=DIRECTION('ref_axis',(1.,0.,0.));
#9703=DIRECTION('center_axis',(0.,1.,0.));
#9704=DIRECTION('ref_axis',(1.,0.,0.));
#9705=DIRECTION('',(-0.447213595499958,0.894427190999916,-5.47678698264203E-17));
#9706=DIRECTION('center_axis',(0.,-1.,0.));
#9707=DIRECTION('ref_axis',(1.,0.,0.));
#9708=DIRECTION('center_axis',(0.,1.,0.));
#9709=DIRECTION('ref_axis',(1.,0.,0.));
#9710=DIRECTION('',(0.,1.,0.));
#9711=DIRECTION('center_axis',(0.,1.,0.));
#9712=DIRECTION('ref_axis',(1.,0.,0.));
#9713=DIRECTION('center_axis',(0.,-1.,0.));
#9714=DIRECTION('ref_axis',(1.,0.,0.));
#9715=DIRECTION('',(-0.707106781186547,0.707106781186548,-8.65956056235493E-17));
#9716=DIRECTION('center_axis',(0.,-1.,0.));
#9717=DIRECTION('ref_axis',(0.,0.,-1.));
#9718=DIRECTION('center_axis',(0.866025403784439,0.,-0.5));
#9719=DIRECTION('ref_axis',(0.5,0.,0.866025403784439));
#9720=DIRECTION('',(-0.5,0.,-0.866025403784439));
#9721=DIRECTION('',(0.,-1.,0.));
#9722=DIRECTION('',(0.5,0.,0.866025403784439));
#9723=DIRECTION('',(0.,-1.,0.));
#9724=DIRECTION('center_axis',(1.20185167898973E-16,0.,-1.));
#9725=DIRECTION('ref_axis',(1.,0.,1.20185167898973E-16));
#9726=DIRECTION('',(-1.,0.,-1.20185167898973E-16));
#9727=DIRECTION('',(0.,-1.,0.));
#9728=DIRECTION('',(1.,0.,1.20185167898973E-16));
#9729=DIRECTION('center_axis',(-0.866025403784439,0.,-0.5));
#9730=DIRECTION('ref_axis',(0.5,0.,-0.866025403784439));
#9731=DIRECTION('',(-0.5,0.,0.866025403784439));
#9732=DIRECTION('',(0.,-1.,0.));
#9733=DIRECTION('',(0.5,0.,-0.866025403784439));
#9734=DIRECTION('center_axis',(-0.866025403784439,0.,0.5));
#9735=DIRECTION('ref_axis',(-0.5,0.,-0.866025403784439));
#9736=DIRECTION('',(0.5,0.,0.866025403784439));
#9737=DIRECTION('',(0.,-1.,0.));
#9738=DIRECTION('',(-0.5,0.,-0.866025403784439));
#9739=DIRECTION('center_axis',(-2.40370335797945E-16,0.,1.));
#9740=DIRECTION('ref_axis',(-1.,0.,-2.40370335797945E-16));
#9741=DIRECTION('',(1.,0.,2.40370335797945E-16));
#9742=DIRECTION('',(0.,-1.,0.));
#9743=DIRECTION('',(-1.,0.,-2.40370335797945E-16));
#9744=DIRECTION('center_axis',(0.866025403784439,0.,0.5));
#9745=DIRECTION('ref_axis',(-0.5,0.,0.866025403784439));
#9746=DIRECTION('',(0.5,0.,-0.866025403784439));
#9747=DIRECTION('',(-0.5,0.,0.866025403784439));
#9748=DIRECTION('center_axis',(0.,1.,0.));
#9749=DIRECTION('ref_axis',(1.,0.,0.));
#9750=DIRECTION('center_axis',(0.,-1.,0.));
#9751=DIRECTION('ref_axis',(0.,0.,-1.));
#9752=DIRECTION('axis',(0.,0.,1.));
#9753=DIRECTION('refdir',(1.,0.,0.));
#9754=DIRECTION('center_axis',(0.,1.,0.));
#9755=DIRECTION('ref_axis',(1.,0.,0.));
#9756=DIRECTION('center_axis',(0.,1.,0.));
#9757=DIRECTION('ref_axis',(1.,0.,0.));
#9758=DIRECTION('',(0.,1.,0.));
#9759=DIRECTION('center_axis',(0.,-1.,0.));
#9760=DIRECTION('ref_axis',(1.,0.,0.));
#9761=DIRECTION('center_axis',(0.,1.,0.));
#9762=DIRECTION('ref_axis',(1.,0.,0.));
#9763=DIRECTION('center_axis',(0.,1.,0.));
#9764=DIRECTION('ref_axis',(1.,0.,0.));
#9765=DIRECTION('',(0.,1.,0.));
#9766=DIRECTION('center_axis',(0.,-1.,0.));
#9767=DIRECTION('ref_axis',(1.,0.,0.));
#9768=DIRECTION('center_axis',(0.,1.,0.));
#9769=DIRECTION('ref_axis',(1.,0.,0.));
#9770=DIRECTION('center_axis',(0.,1.,0.));
#9771=DIRECTION('ref_axis',(1.,0.,0.));
#9772=DIRECTION('',(0.,1.,0.));
#9773=DIRECTION('center_axis',(0.,-1.,0.));
#9774=DIRECTION('ref_axis',(1.,0.,0.));
#9775=DIRECTION('center_axis',(0.,1.,0.));
#9776=DIRECTION('ref_axis',(1.,0.,0.));
#9777=DIRECTION('center_axis',(0.,1.,0.));
#9778=DIRECTION('ref_axis',(1.,0.,0.));
#9779=DIRECTION('',(0.,1.,0.));
#9780=DIRECTION('center_axis',(0.,-1.,0.));
#9781=DIRECTION('ref_axis',(1.,0.,0.));
#9782=DIRECTION('center_axis',(0.,1.,0.));
#9783=DIRECTION('ref_axis',(-1.,0.,0.));
#9784=DIRECTION('',(-1.,0.,0.));
#9785=DIRECTION('',(0.,0.,1.));
#9786=DIRECTION('',(-1.,0.,0.));
#9787=DIRECTION('',(0.,0.,1.));
#9788=DIRECTION('center_axis',(1.,0.,0.));
#9789=DIRECTION('ref_axis',(0.,1.,0.));
#9790=DIRECTION('',(0.,1.,0.));
#9791=DIRECTION('',(0.,1.,0.));
#9792=DIRECTION('',(0.,0.,1.));
#9793=DIRECTION('center_axis',(0.,-1.,0.));
#9794=DIRECTION('ref_axis',(1.,0.,0.));
#9795=DIRECTION('',(1.,0.,0.));
#9796=DIRECTION('',(1.,0.,0.));
#9797=DIRECTION('',(0.,0.,1.));
#9798=DIRECTION('center_axis',(-1.,0.,0.));
#9799=DIRECTION('ref_axis',(0.,-1.,0.));
#9800=DIRECTION('',(0.,-1.,0.));
#9801=DIRECTION('',(0.,-1.,0.));
#9802=DIRECTION('center_axis',(0.,0.,1.));
#9803=DIRECTION('ref_axis',(1.,0.,0.));
#9804=DIRECTION('center_axis',(0.,0.,1.));
#9805=DIRECTION('ref_axis',(1.,0.,0.));
#9806=DIRECTION('axis',(0.,0.,1.));
#9807=DIRECTION('refdir',(1.,0.,0.));
#9808=DIRECTION('center_axis',(0.,1.,0.));
#9809=DIRECTION('ref_axis',(1.,0.,0.));
#9810=DIRECTION('center_axis',(0.,1.,0.));
#9811=DIRECTION('ref_axis',(1.,0.,0.));
#9812=DIRECTION('',(0.707106781186548,-0.707106781186547,-8.65956056235494E-17));
#9813=DIRECTION('center_axis',(0.,-1.,0.));
#9814=DIRECTION('ref_axis',(1.,0.,0.));
#9815=DIRECTION('center_axis',(0.,1.,0.));
#9816=DIRECTION('ref_axis',(1.,0.,0.));
#9817=DIRECTION('',(0.,-1.,0.));
#9818=DIRECTION('center_axis',(0.,-1.,0.));
#9819=DIRECTION('ref_axis',(1.,0.,0.));
#9820=DIRECTION('center_axis',(0.,1.,0.));
#9821=DIRECTION('ref_axis',(1.,0.,0.));
#9822=DIRECTION('center_axis',(0.,1.,0.));
#9823=DIRECTION('ref_axis',(1.,0.,0.));
#9824=DIRECTION('center_axis',(0.,1.,0.));
#9825=DIRECTION('ref_axis',(1.,0.,0.));
#9826=DIRECTION('',(0.,-1.,0.));
#9827=DIRECTION('center_axis',(0.,1.,0.));
#9828=DIRECTION('ref_axis',(1.,0.,0.));
#9829=DIRECTION('center_axis',(0.,1.,0.));
#9830=DIRECTION('ref_axis',(1.,0.,0.));
#9831=DIRECTION('axis',(0.,0.,1.));
#9832=DIRECTION('refdir',(1.,0.,0.));
#9833=DIRECTION('center_axis',(0.,0.,1.));
#9834=DIRECTION('ref_axis',(1.,0.,0.));
#9835=DIRECTION('center_axis',(0.,0.,1.));
#9836=DIRECTION('ref_axis',(1.,0.,0.));
#9837=DIRECTION('',(0.,0.,1.));
#9838=DIRECTION('center_axis',(0.,0.,-1.));
#9839=DIRECTION('ref_axis',(1.,0.,0.));
#9840=DIRECTION('center_axis',(0.,0.,1.));
#9841=DIRECTION('ref_axis',(1.,0.,0.));
#9842=DIRECTION('center_axis',(0.,0.,1.));
#9843=DIRECTION('ref_axis',(1.,0.,0.));
#9844=DIRECTION('',(0.,0.,1.));
#9845=DIRECTION('center_axis',(0.,0.,-1.));
#9846=DIRECTION('ref_axis',(1.,0.,0.));
#9847=DIRECTION('center_axis',(0.,1.,0.));
#9848=DIRECTION('ref_axis',(-1.,0.,0.));
#9849=DIRECTION('',(-1.,0.,0.));
#9850=DIRECTION('',(0.,0.,1.));
#9851=DIRECTION('',(-1.,0.,0.));
#9852=DIRECTION('',(0.,0.,1.));
#9853=DIRECTION('center_axis',(1.,0.,0.));
#9854=DIRECTION('ref_axis',(0.,1.,0.));
#9855=DIRECTION('',(0.,1.,0.));
#9856=DIRECTION('',(0.,1.,0.));
#9857=DIRECTION('',(0.,0.,1.));
#9858=DIRECTION('center_axis',(0.,-1.,0.));
#9859=DIRECTION('ref_axis',(1.,0.,0.));
#9860=DIRECTION('',(1.,0.,0.));
#9861=DIRECTION('',(1.,0.,0.));
#9862=DIRECTION('',(0.,0.,1.));
#9863=DIRECTION('center_axis',(-1.,0.,0.));
#9864=DIRECTION('ref_axis',(0.,-1.,0.));
#9865=DIRECTION('',(0.,-1.,0.));
#9866=DIRECTION('',(0.,-1.,0.));
#9867=DIRECTION('center_axis',(0.,0.,1.));
#9868=DIRECTION('ref_axis',(1.,0.,0.));
#9869=DIRECTION('center_axis',(0.,0.,1.));
#9870=DIRECTION('ref_axis',(1.,0.,0.));
#9871=DIRECTION('axis',(0.,0.,1.));
#9872=DIRECTION('refdir',(1.,0.,0.));
#9873=DIRECTION('center_axis',(0.,1.,0.));
#9874=DIRECTION('ref_axis',(-1.,0.,0.));
#9875=DIRECTION('',(-1.,0.,0.));
#9876=DIRECTION('',(0.,0.,1.));
#9877=DIRECTION('',(-1.,0.,0.));
#9878=DIRECTION('',(0.,0.,1.));
#9879=DIRECTION('center_axis',(1.,0.,0.));
#9880=DIRECTION('ref_axis',(0.,1.,0.));
#9881=DIRECTION('',(0.,1.,0.));
#9882=DIRECTION('',(0.,1.,0.));
#9883=DIRECTION('',(0.,0.,1.));
#9884=DIRECTION('center_axis',(0.,-1.,0.));
#9885=DIRECTION('ref_axis',(1.,0.,0.));
#9886=DIRECTION('',(1.,0.,0.));
#9887=DIRECTION('',(1.,0.,0.));
#9888=DIRECTION('',(0.,0.,1.));
#9889=DIRECTION('center_axis',(-1.,0.,0.));
#9890=DIRECTION('ref_axis',(0.,-1.,0.));
#9891=DIRECTION('',(0.,-1.,0.));
#9892=DIRECTION('',(0.,-1.,0.));
#9893=DIRECTION('center_axis',(0.,0.,1.));
#9894=DIRECTION('ref_axis',(1.,0.,0.));
#9895=DIRECTION('center_axis',(0.,0.,1.));
#9896=DIRECTION('ref_axis',(1.,0.,0.));
#9897=DIRECTION('axis',(0.,0.,1.));
#9898=DIRECTION('refdir',(1.,0.,0.));
#9899=DIRECTION('center_axis',(0.,1.,0.));
#9900=DIRECTION('ref_axis',(-1.,0.,0.));
#9901=DIRECTION('',(-1.,0.,0.));
#9902=DIRECTION('',(0.,0.,1.));
#9903=DIRECTION('',(-1.,0.,0.));
#9904=DIRECTION('',(0.,0.,1.));
#9905=DIRECTION('center_axis',(1.,0.,0.));
#9906=DIRECTION('ref_axis',(0.,1.,0.));
#9907=DIRECTION('',(0.,1.,0.));
#9908=DIRECTION('',(0.,1.,0.));
#9909=DIRECTION('',(0.,0.,1.));
#9910=DIRECTION('center_axis',(0.,-1.,0.));
#9911=DIRECTION('ref_axis',(1.,0.,0.));
#9912=DIRECTION('',(1.,0.,0.));
#9913=DIRECTION('',(1.,0.,0.));
#9914=DIRECTION('',(0.,0.,1.));
#9915=DIRECTION('center_axis',(-1.,0.,0.));
#9916=DIRECTION('ref_axis',(0.,-1.,0.));
#9917=DIRECTION('',(0.,-1.,0.));
#9918=DIRECTION('',(0.,-1.,0.));
#9919=DIRECTION('center_axis',(0.,0.,1.));
#9920=DIRECTION('ref_axis',(1.,0.,0.));
#9921=DIRECTION('center_axis',(0.,0.,1.));
#9922=DIRECTION('ref_axis',(1.,0.,0.));
#9923=DIRECTION('axis',(0.,0.,1.));
#9924=DIRECTION('refdir',(1.,0.,0.));
#9925=DIRECTION('center_axis',(0.,0.,1.));
#9926=DIRECTION('ref_axis',(1.,0.,0.));
#9927=DIRECTION('center_axis',(0.,0.,1.));
#9928=DIRECTION('ref_axis',(1.,0.,0.));
#9929=DIRECTION('',(0.,0.,1.));
#9930=DIRECTION('center_axis',(0.,0.,-1.));
#9931=DIRECTION('ref_axis',(1.,0.,0.));
#9932=DIRECTION('center_axis',(0.,0.,1.));
#9933=DIRECTION('ref_axis',(1.,0.,0.));
#9934=DIRECTION('center_axis',(0.,0.,1.));
#9935=DIRECTION('ref_axis',(1.,0.,0.));
#9936=DIRECTION('',(0.,0.,1.));
#9937=DIRECTION('center_axis',(0.,0.,-1.));
#9938=DIRECTION('ref_axis',(1.,0.,0.));
#9939=DIRECTION('center_axis',(0.,1.,0.));
#9940=DIRECTION('ref_axis',(-1.,0.,0.));
#9941=DIRECTION('',(-1.,0.,0.));
#9942=DIRECTION('',(0.,0.,1.));
#9943=DIRECTION('',(-1.,0.,0.));
#9944=DIRECTION('',(0.,0.,1.));
#9945=DIRECTION('center_axis',(1.,0.,0.));
#9946=DIRECTION('ref_axis',(0.,1.,0.));
#9947=DIRECTION('',(0.,1.,0.));
#9948=DIRECTION('',(0.,1.,0.));
#9949=DIRECTION('',(0.,0.,1.));
#9950=DIRECTION('center_axis',(0.,-1.,0.));
#9951=DIRECTION('ref_axis',(1.,0.,0.));
#9952=DIRECTION('',(1.,0.,0.));
#9953=DIRECTION('',(1.,0.,0.));
#9954=DIRECTION('',(0.,0.,1.));
#9955=DIRECTION('center_axis',(-1.,0.,0.));
#9956=DIRECTION('ref_axis',(0.,-1.,0.));
#9957=DIRECTION('',(0.,-1.,0.));
#9958=DIRECTION('',(0.,-1.,0.));
#9959=DIRECTION('center_axis',(0.,0.,1.));
#9960=DIRECTION('ref_axis',(1.,0.,0.));
#9961=DIRECTION('center_axis',(0.,0.,1.));
#9962=DIRECTION('ref_axis',(1.,0.,0.));
#9963=DIRECTION('axis',(0.,0.,1.));
#9964=DIRECTION('refdir',(1.,0.,0.));
#9965=DIRECTION('center_axis',(0.,1.,0.));
#9966=DIRECTION('ref_axis',(-1.,0.,0.));
#9967=DIRECTION('',(-1.,0.,0.));
#9968=DIRECTION('',(0.,0.,1.));
#9969=DIRECTION('',(-1.,0.,0.));
#9970=DIRECTION('',(0.,0.,1.));
#9971=DIRECTION('center_axis',(1.,0.,0.));
#9972=DIRECTION('ref_axis',(0.,1.,0.));
#9973=DIRECTION('',(0.,1.,0.));
#9974=DIRECTION('',(0.,1.,0.));
#9975=DIRECTION('',(0.,0.,1.));
#9976=DIRECTION('center_axis',(0.,-1.,0.));
#9977=DIRECTION('ref_axis',(1.,0.,0.));
#9978=DIRECTION('',(1.,0.,0.));
#9979=DIRECTION('',(1.,0.,0.));
#9980=DIRECTION('',(0.,0.,1.));
#9981=DIRECTION('center_axis',(-1.,0.,0.));
#9982=DIRECTION('ref_axis',(0.,-1.,0.));
#9983=DIRECTION('',(0.,-1.,0.));
#9984=DIRECTION('',(0.,-1.,0.));
#9985=DIRECTION('center_axis',(0.,0.,1.));
#9986=DIRECTION('ref_axis',(1.,0.,0.));
#9987=DIRECTION('center_axis',(0.,0.,1.));
#9988=DIRECTION('ref_axis',(1.,0.,0.));
#9989=DIRECTION('axis',(0.,0.,1.));
#9990=DIRECTION('refdir',(1.,0.,0.));
#9991=DIRECTION('center_axis',(0.,1.,0.));
#9992=DIRECTION('ref_axis',(-1.,0.,0.));
#9993=DIRECTION('',(-1.,0.,0.));
#9994=DIRECTION('',(0.,0.,1.));
#9995=DIRECTION('',(-1.,0.,0.));
#9996=DIRECTION('',(0.,0.,1.));
#9997=DIRECTION('center_axis',(1.,0.,0.));
#9998=DIRECTION('ref_axis',(0.,1.,0.));
#9999=DIRECTION('',(0.,1.,0.));
#10000=DIRECTION('',(0.,1.,0.));
#10001=DIRECTION('',(0.,0.,1.));
#10002=DIRECTION('center_axis',(0.,-1.,0.));
#10003=DIRECTION('ref_axis',(1.,0.,0.));
#10004=DIRECTION('',(1.,0.,0.));
#10005=DIRECTION('',(1.,0.,0.));
#10006=DIRECTION('',(0.,0.,1.));
#10007=DIRECTION('center_axis',(-1.,0.,0.));
#10008=DIRECTION('ref_axis',(0.,-1.,0.));
#10009=DIRECTION('',(0.,-1.,0.));
#10010=DIRECTION('',(0.,-1.,0.));
#10011=DIRECTION('center_axis',(0.,0.,1.));
#10012=DIRECTION('ref_axis',(1.,0.,0.));
#10013=DIRECTION('center_axis',(0.,0.,1.));
#10014=DIRECTION('ref_axis',(1.,0.,0.));
#10015=DIRECTION('axis',(0.,0.,1.));
#10016=DIRECTION('refdir',(1.,0.,0.));
#10017=DIRECTION('axis',(0.,0.,1.));
#10018=DIRECTION('refdir',(1.,0.,0.));
#10019=DIRECTION('center_axis',(0.,1.,0.));
#10020=DIRECTION('ref_axis',(1.,0.,0.));
#10021=DIRECTION('center_axis',(0.,-1.,0.));
#10022=DIRECTION('ref_axis',(1.,0.,0.));
#10023=DIRECTION('',(0.,-1.,0.));
#10024=DIRECTION('center_axis',(0.,-1.,0.));
#10025=DIRECTION('ref_axis',(1.,0.,0.));
#10026=DIRECTION('center_axis',(0.,1.,0.));
#10027=DIRECTION('ref_axis',(1.,0.,0.));
#10028=DIRECTION('center_axis',(0.,1.,0.));
#10029=DIRECTION('ref_axis',(1.,0.,0.));
#10030=DIRECTION('',(0.,-1.,0.));
#10031=DIRECTION('center_axis',(0.,1.,0.));
#10032=DIRECTION('ref_axis',(1.,0.,0.));
#10033=DIRECTION('center_axis',(0.,1.,0.));
#10034=DIRECTION('ref_axis',(1.,0.,0.));
#10035=DIRECTION('center_axis',(0.,1.,0.));
#10036=DIRECTION('ref_axis',(1.,0.,0.));
#10037=DIRECTION('axis',(0.,0.,1.));
#10038=DIRECTION('refdir',(1.,0.,0.));
#10039=DIRECTION('center_axis',(0.,1.,0.));
#10040=DIRECTION('ref_axis',(1.,0.,0.));
#10041=DIRECTION('center_axis',(0.,-1.,0.));
#10042=DIRECTION('ref_axis',(1.,0.,0.));
#10043=DIRECTION('',(0.,-1.,0.));
#10044=DIRECTION('center_axis',(0.,-1.,0.));
#10045=DIRECTION('ref_axis',(1.,0.,0.));
#10046=DIRECTION('center_axis',(0.,1.,0.));
#10047=DIRECTION('ref_axis',(1.,0.,0.));
#10048=DIRECTION('center_axis',(0.,1.,0.));
#10049=DIRECTION('ref_axis',(1.,0.,0.));
#10050=DIRECTION('center_axis',(0.,1.,0.));
#10051=DIRECTION('ref_axis',(1.,0.,0.));
#10052=DIRECTION('',(0.,-1.,0.));
#10053=DIRECTION('center_axis',(0.,-1.,0.));
#10054=DIRECTION('ref_axis',(1.,0.,0.));
#10055=DIRECTION('center_axis',(0.,1.,0.));
#10056=DIRECTION('ref_axis',(1.,0.,0.));
#10057=DIRECTION('center_axis',(0.,1.,0.));
#10058=DIRECTION('ref_axis',(1.,0.,0.));
#10059=DIRECTION('',(0.,-1.,0.));
#10060=DIRECTION('center_axis',(0.,1.,0.));
#10061=DIRECTION('ref_axis',(1.,0.,0.));
#10062=DIRECTION('center_axis',(0.,1.,0.));
#10063=DIRECTION('ref_axis',(1.,0.,0.));
#10064=DIRECTION('center_axis',(0.,1.,0.));
#10065=DIRECTION('ref_axis',(1.,0.,0.));
#10066=DIRECTION('axis',(0.,0.,1.));
#10067=DIRECTION('refdir',(1.,0.,0.));
#10068=DIRECTION('center_axis',(0.,1.,0.));
#10069=DIRECTION('ref_axis',(1.,0.,0.));
#10070=DIRECTION('center_axis',(0.,-1.,0.));
#10071=DIRECTION('ref_axis',(1.,0.,0.));
#10072=DIRECTION('',(0.,1.,0.));
#10073=DIRECTION('center_axis',(0.,1.,0.));
#10074=DIRECTION('ref_axis',(1.,0.,0.));
#10075=DIRECTION('center_axis',(0.,1.,0.));
#10076=DIRECTION('ref_axis',(1.,0.,0.));
#10077=DIRECTION('center_axis',(0.,-1.,0.));
#10078=DIRECTION('ref_axis',(1.,0.,0.));
#10079=DIRECTION('center_axis',(0.,1.,0.));
#10080=DIRECTION('ref_axis',(1.,0.,0.));
#10081=DIRECTION('',(0.,-1.,0.));
#10082=DIRECTION('center_axis',(0.,-1.,0.));
#10083=DIRECTION('ref_axis',(1.,0.,0.));
#10084=DIRECTION('center_axis',(0.,1.,0.));
#10085=DIRECTION('ref_axis',(1.,0.,0.));
#10086=DIRECTION('center_axis',(0.,1.,0.));
#10087=DIRECTION('ref_axis',(1.,0.,0.));
#10088=DIRECTION('',(0.,-1.,0.));
#10089=DIRECTION('center_axis',(0.,1.,0.));
#10090=DIRECTION('ref_axis',(1.,0.,0.));
#10091=DIRECTION('center_axis',(0.,1.,0.));
#10092=DIRECTION('ref_axis',(1.,0.,0.));
#10093=DIRECTION('center_axis',(0.,1.,0.));
#10094=DIRECTION('ref_axis',(1.,0.,0.));
#10095=DIRECTION('axis',(0.,0.,1.));
#10096=DIRECTION('refdir',(1.,0.,0.));
#10097=DIRECTION('center_axis',(0.,1.,0.));
#10098=DIRECTION('ref_axis',(1.,0.,0.));
#10099=DIRECTION('center_axis',(0.,-1.,0.));
#10100=DIRECTION('ref_axis',(1.,0.,0.));
#10101=DIRECTION('',(0.,-1.,0.));
#10102=DIRECTION('center_axis',(0.,-1.,0.));
#10103=DIRECTION('ref_axis',(1.,0.,0.));
#10104=DIRECTION('center_axis',(0.,1.,0.));
#10105=DIRECTION('ref_axis',(1.,0.,0.));
#10106=DIRECTION('center_axis',(0.,-1.,0.));
#10107=DIRECTION('ref_axis',(1.,0.,0.));
#10108=DIRECTION('center_axis',(0.,1.,0.));
#10109=DIRECTION('ref_axis',(1.,0.,0.));
#10110=DIRECTION('center_axis',(0.,-1.,0.));
#10111=DIRECTION('ref_axis',(1.,0.,0.));
#10112=DIRECTION('',(0.,-1.,0.));
#10113=DIRECTION('center_axis',(0.,1.,0.));
#10114=DIRECTION('ref_axis',(1.,0.,0.));
#10115=DIRECTION('center_axis',(0.,1.,0.));
#10116=DIRECTION('ref_axis',(1.,0.,0.));
#10117=DIRECTION('',(0.,-1.,0.));
#10118=DIRECTION('center_axis',(0.,1.,0.));
#10119=DIRECTION('ref_axis',(1.,0.,0.));
#10120=DIRECTION('center_axis',(0.,1.,0.));
#10121=DIRECTION('ref_axis',(1.,0.,0.));
#10122=DIRECTION('center_axis',(0.,1.,0.));
#10123=DIRECTION('ref_axis',(1.,0.,0.));
#10124=DIRECTION('axis',(0.,0.,1.));
#10125=DIRECTION('refdir',(1.,0.,0.));
#10126=DIRECTION('center_axis',(0.,1.,0.));
#10127=DIRECTION('ref_axis',(1.,0.,0.));
#10128=DIRECTION('center_axis',(0.,-1.,0.));
#10129=DIRECTION('ref_axis',(1.,0.,0.));
#10130=DIRECTION('',(0.,1.,0.));
#10131=DIRECTION('center_axis',(0.,-1.,0.));
#10132=DIRECTION('ref_axis',(1.,0.,0.));
#10133=DIRECTION('center_axis',(0.,1.,0.));
#10134=DIRECTION('ref_axis',(1.,0.,0.));
#10135=DIRECTION('center_axis',(0.,-1.,0.));
#10136=DIRECTION('ref_axis',(1.,0.,0.));
#10137=DIRECTION('center_axis',(0.,1.,0.));
#10138=DIRECTION('ref_axis',(1.,0.,0.));
#10139=DIRECTION('center_axis',(0.,-1.,0.));
#10140=DIRECTION('ref_axis',(1.,0.,0.));
#10141=DIRECTION('',(0.,-1.,0.));
#10142=DIRECTION('center_axis',(0.,1.,0.));
#10143=DIRECTION('ref_axis',(1.,0.,0.));
#10144=DIRECTION('center_axis',(0.,1.,0.));
#10145=DIRECTION('ref_axis',(1.,0.,0.));
#10146=DIRECTION('',(0.,-1.,0.));
#10147=DIRECTION('center_axis',(0.,1.,0.));
#10148=DIRECTION('ref_axis',(1.,0.,0.));
#10149=DIRECTION('center_axis',(0.,1.,0.));
#10150=DIRECTION('ref_axis',(1.,0.,0.));
#10151=DIRECTION('center_axis',(0.,1.,0.));
#10152=DIRECTION('ref_axis',(1.,0.,0.));
#10153=DIRECTION('axis',(0.,0.,1.));
#10154=DIRECTION('refdir',(1.,0.,0.));
#10155=DIRECTION('center_axis',(0.,1.,0.));
#10156=DIRECTION('ref_axis',(1.,0.,0.));
#10157=DIRECTION('center_axis',(0.,1.,0.));
#10158=DIRECTION('ref_axis',(1.,0.,0.));
#10159=DIRECTION('',(0.,1.,0.));
#10160=DIRECTION('center_axis',(0.,-1.,0.));
#10161=DIRECTION('ref_axis',(1.,0.,0.));
#10162=DIRECTION('center_axis',(0.,1.,0.));
#10163=DIRECTION('ref_axis',(1.,0.,0.));
#10164=DIRECTION('center_axis',(0.,1.,0.));
#10165=DIRECTION('ref_axis',(1.,0.,0.));
#10166=DIRECTION('center_axis',(0.,1.,0.));
#10167=DIRECTION('ref_axis',(1.,0.,0.));
#10168=DIRECTION('',(0.,1.,0.));
#10169=DIRECTION('center_axis',(0.,1.,0.));
#10170=DIRECTION('ref_axis',(1.,0.,0.));
#10171=DIRECTION('center_axis',(0.,1.,0.));
#10172=DIRECTION('ref_axis',(1.,0.,0.));
#10173=DIRECTION('center_axis',(0.,1.,0.));
#10174=DIRECTION('ref_axis',(1.,0.,0.));
#10175=DIRECTION('center_axis',(0.,1.,0.));
#10176=DIRECTION('ref_axis',(1.,0.,0.));
#10177=DIRECTION('',(0.,-1.,0.));
#10178=DIRECTION('center_axis',(0.,1.,0.));
#10179=DIRECTION('ref_axis',(1.,0.,0.));
#10180=DIRECTION('center_axis',(0.,1.,0.));
#10181=DIRECTION('ref_axis',(1.,0.,0.));
#10182=DIRECTION('center_axis',(0.,1.,0.));
#10183=DIRECTION('ref_axis',(1.,0.,0.));
#10184=DIRECTION('axis',(0.,0.,1.));
#10185=DIRECTION('refdir',(1.,0.,0.));
#10186=DIRECTION('center_axis',(0.,0.,1.));
#10187=DIRECTION('ref_axis',(1.,0.,0.));
#10188=DIRECTION('center_axis',(0.,0.,1.));
#10189=DIRECTION('ref_axis',(1.,0.,0.));
#10190=DIRECTION('',(0.,0.,1.));
#10191=DIRECTION('center_axis',(0.,0.,-1.));
#10192=DIRECTION('ref_axis',(1.,0.,0.));
#10193=DIRECTION('center_axis',(0.,0.,1.));
#10194=DIRECTION('ref_axis',(1.,0.,0.));
#10195=DIRECTION('center_axis',(0.,0.,1.));
#10196=DIRECTION('ref_axis',(1.,0.,0.));
#10197=DIRECTION('center_axis',(0.,0.,1.));
#10198=DIRECTION('ref_axis',(1.,0.,0.));
#10199=DIRECTION('center_axis',(0.,0.,1.));
#10200=DIRECTION('ref_axis',(1.,0.,0.));
#10201=DIRECTION('',(0.,0.,1.));
#10202=DIRECTION('center_axis',(0.,0.,-1.));
#10203=DIRECTION('ref_axis',(1.,0.,0.));
#10204=DIRECTION('center_axis',(0.,0.,1.));
#10205=DIRECTION('ref_axis',(1.,0.,0.));
#10206=DIRECTION('center_axis',(0.,0.,1.));
#10207=DIRECTION('ref_axis',(1.,0.,0.));
#10208=DIRECTION('center_axis',(0.,0.,1.));
#10209=DIRECTION('ref_axis',(1.,0.,0.));
#10210=DIRECTION('center_axis',(0.,0.,1.));
#10211=DIRECTION('ref_axis',(1.,0.,0.));
#10212=DIRECTION('',(0.,0.,1.));
#10213=DIRECTION('center_axis',(0.,0.,1.));
#10214=DIRECTION('ref_axis',(1.,0.,0.));
#10215=DIRECTION('center_axis',(0.,0.,1.));
#10216=DIRECTION('ref_axis',(1.,0.,0.));
#10217=DIRECTION('',(0.,0.,1.));
#10218=DIRECTION('center_axis',(0.,1.,0.));
#10219=DIRECTION('ref_axis',(1.,0.,0.));
#10220=DIRECTION('center_axis',(0.,1.,0.));
#10221=DIRECTION('ref_axis',(1.,0.,0.));
#10222=DIRECTION('',(0.,1.,0.));
#10223=DIRECTION('center_axis',(0.,-1.,0.));
#10224=DIRECTION('ref_axis',(1.,0.,0.));
#10225=DIRECTION('center_axis',(0.,1.,0.));
#10226=DIRECTION('ref_axis',(-1.,0.,0.));
#10227=DIRECTION('',(-1.,0.,0.));
#10228=DIRECTION('',(0.,0.,1.));
#10229=DIRECTION('',(-1.,0.,0.));
#10230=DIRECTION('',(0.,0.,1.));
#10231=DIRECTION('center_axis',(1.,0.,0.));
#10232=DIRECTION('ref_axis',(0.,1.,0.));
#10233=DIRECTION('',(0.,1.,0.));
#10234=DIRECTION('',(0.,1.,0.));
#10235=DIRECTION('',(0.,0.,1.));
#10236=DIRECTION('center_axis',(0.,-1.,0.));
#10237=DIRECTION('ref_axis',(1.,0.,0.));
#10238=DIRECTION('',(1.,0.,0.));
#10239=DIRECTION('',(1.,0.,0.));
#10240=DIRECTION('',(0.,0.,1.));
#10241=DIRECTION('center_axis',(-1.,0.,0.));
#10242=DIRECTION('ref_axis',(0.,-1.,0.));
#10243=DIRECTION('',(0.,-1.,0.));
#10244=DIRECTION('',(0.,-1.,0.));
#10245=DIRECTION('center_axis',(0.,0.,1.));
#10246=DIRECTION('ref_axis',(1.,0.,0.));
#10247=DIRECTION('center_axis',(0.,0.,1.));
#10248=DIRECTION('ref_axis',(1.,0.,0.));
#10249=DIRECTION('axis',(0.,0.,1.));
#10250=DIRECTION('refdir',(1.,0.,0.));
#10251=DIRECTION('center_axis',(0.,1.,0.));
#10252=DIRECTION('ref_axis',(1.,0.,0.));
#10253=DIRECTION('center_axis',(0.,-1.,0.));
#10254=DIRECTION('ref_axis',(1.,0.,0.));
#10255=DIRECTION('',(0.,-1.,0.));
#10256=DIRECTION('center_axis',(0.,-1.,0.));
#10257=DIRECTION('ref_axis',(1.,0.,0.));
#10258=DIRECTION('center_axis',(0.,1.,0.));
#10259=DIRECTION('ref_axis',(1.,0.,0.));
#10260=DIRECTION('center_axis',(0.,1.,0.));
#10261=DIRECTION('ref_axis',(1.,0.,0.));
#10262=DIRECTION('',(0.,-1.,0.));
#10263=DIRECTION('center_axis',(0.,1.,0.));
#10264=DIRECTION('ref_axis',(1.,0.,0.));
#10265=DIRECTION('center_axis',(0.,1.,0.));
#10266=DIRECTION('ref_axis',(1.,0.,0.));
#10267=DIRECTION('center_axis',(0.,1.,0.));
#10268=DIRECTION('ref_axis',(1.,0.,0.));
#10269=DIRECTION('axis',(0.,0.,1.));
#10270=DIRECTION('refdir',(1.,0.,0.));
#10271=DIRECTION('center_axis',(0.,1.,0.));
#10272=DIRECTION('ref_axis',(1.,0.,0.));
#10273=DIRECTION('center_axis',(0.,-1.,0.));
#10274=DIRECTION('ref_axis',(1.,0.,0.));
#10275=DIRECTION('',(0.,-1.,0.));
#10276=DIRECTION('center_axis',(0.,-1.,0.));
#10277=DIRECTION('ref_axis',(1.,0.,0.));
#10278=DIRECTION('center_axis',(0.,1.,0.));
#10279=DIRECTION('ref_axis',(1.,0.,0.));
#10280=DIRECTION('center_axis',(0.,1.,0.));
#10281=DIRECTION('ref_axis',(1.,0.,0.));
#10282=DIRECTION('',(0.,-1.,0.));
#10283=DIRECTION('center_axis',(0.,1.,0.));
#10284=DIRECTION('ref_axis',(1.,0.,0.));
#10285=DIRECTION('center_axis',(0.,1.,0.));
#10286=DIRECTION('ref_axis',(1.,0.,0.));
#10287=DIRECTION('center_axis',(0.,1.,0.));
#10288=DIRECTION('ref_axis',(1.,0.,0.));
#10289=DIRECTION('axis',(0.,0.,1.));
#10290=DIRECTION('refdir',(1.,0.,0.));
#10291=DIRECTION('axis',(0.,0.,1.));
#10292=DIRECTION('refdir',(1.,0.,0.));
#10293=DIRECTION('center_axis',(0.,-1.,0.));
#10294=DIRECTION('ref_axis',(0.,0.,-1.));
#10295=DIRECTION('center_axis',(0.,-1.,0.));
#10296=DIRECTION('ref_axis',(1.,0.,0.));
#10297=DIRECTION('center_axis',(0.,-1.,0.));
#10298=DIRECTION('ref_axis',(1.,0.,0.));
#10299=DIRECTION('center_axis',(1.,0.,1.22464679914735E-16));
#10300=DIRECTION('ref_axis',(-1.22464679914735E-16,0.,1.));
#10301=DIRECTION('center_axis',(0.,1.,0.));
#10302=DIRECTION('ref_axis',(1.,0.,0.));
#10303=DIRECTION('center_axis',(0.,1.,0.));
#10304=DIRECTION('ref_axis',(1.,0.,0.));
#10305=DIRECTION('center_axis',(0.,-1.,0.));
#10306=DIRECTION('ref_axis',(1.,0.,0.));
#10307=DIRECTION('',(0.,1.,0.));
#10308=DIRECTION('center_axis',(0.,-1.,0.));
#10309=DIRECTION('ref_axis',(1.,0.,0.));
#10310=DIRECTION('center_axis',(0.,-1.,0.));
#10311=DIRECTION('ref_axis',(1.,0.,0.));
#10312=DIRECTION('center_axis',(0.,-1.,0.));
#10313=DIRECTION('ref_axis',(1.,0.,0.));
#10314=DIRECTION('',(0.,1.,0.));
#10315=DIRECTION('center_axis',(0.,-1.,0.));
#10316=DIRECTION('ref_axis',(1.,0.,0.));
#10317=DIRECTION('center_axis',(0.,1.,0.));
#10318=DIRECTION('ref_axis',(1.,0.,0.));
#10319=DIRECTION('',(-0.707106781186547,0.707106781186548,-8.65956056235493E-17));
#10320=DIRECTION('center_axis',(0.,-1.,0.));
#10321=DIRECTION('ref_axis',(1.,0.,0.));
#10322=DIRECTION('center_axis',(0.,1.,0.));
#10323=DIRECTION('ref_axis',(0.,0.,1.));
#10324=DIRECTION('center_axis',(0.,-1.,0.));
#10325=DIRECTION('ref_axis',(1.,0.,0.));
#10326=DIRECTION('center_axis',(0.,-1.,0.));
#10327=DIRECTION('ref_axis',(1.,0.,0.));
#10328=DIRECTION('',(0.,1.,0.));
#10329=DIRECTION('center_axis',(0.,-1.,0.));
#10330=DIRECTION('ref_axis',(0.,0.,-1.));
#10331=DIRECTION('center_axis',(0.,-1.,0.));
#10332=DIRECTION('ref_axis',(1.,0.,0.));
#10333=DIRECTION('center_axis',(0.,-1.,0.));
#10334=DIRECTION('ref_axis',(1.,0.,0.));
#10335=DIRECTION('',(0.707106781186547,0.707106781186548,8.65956056235493E-17));
#10336=DIRECTION('axis',(0.,0.,1.));
#10337=DIRECTION('refdir',(1.,0.,0.));
#10338=DIRECTION('center_axis',(0.,-1.,0.));
#10339=DIRECTION('ref_axis',(0.,0.,-1.));
#10340=DIRECTION('center_axis',(0.,-1.,0.));
#10341=DIRECTION('ref_axis',(1.,0.,0.));
#10342=DIRECTION('center_axis',(0.,-1.,0.));
#10343=DIRECTION('ref_axis',(1.,0.,0.));
#10344=DIRECTION('center_axis',(1.,0.,1.22464679914735E-16));
#10345=DIRECTION('ref_axis',(-1.22464679914735E-16,0.,1.));
#10346=DIRECTION('center_axis',(0.,1.,0.));
#10347=DIRECTION('ref_axis',(1.,0.,0.));
#10348=DIRECTION('center_axis',(0.,1.,0.));
#10349=DIRECTION('ref_axis',(1.,0.,0.));
#10350=DIRECTION('center_axis',(0.,-1.,0.));
#10351=DIRECTION('ref_axis',(1.,0.,0.));
#10352=DIRECTION('center_axis',(0.,-1.,0.));
#10353=DIRECTION('ref_axis',(1.,0.,0.));
#10354=DIRECTION('',(0.,1.,0.));
#10355=DIRECTION('center_axis',(0.,1.,0.));
#10356=DIRECTION('ref_axis',(0.,0.,1.));
#10357=DIRECTION('center_axis',(0.,-1.,0.));
#10358=DIRECTION('ref_axis',(1.,0.,0.));
#10359=DIRECTION('center_axis',(0.,-1.,0.));
#10360=DIRECTION('ref_axis',(1.,0.,0.));
#10361=DIRECTION('center_axis',(0.,-1.,0.));
#10362=DIRECTION('ref_axis',(1.,0.,0.));
#10363=DIRECTION('center_axis',(0.,-1.,0.));
#10364=DIRECTION('ref_axis',(1.,0.,0.));
#10365=DIRECTION('',(0.707106781186548,0.707106781186547,8.65956056235494E-17));
#10366=DIRECTION('center_axis',(0.,-1.,0.));
#10367=DIRECTION('ref_axis',(1.,0.,0.));
#10368=DIRECTION('center_axis',(0.,-1.,0.));
#10369=DIRECTION('ref_axis',(1.,0.,0.));
#10370=DIRECTION('',(0.,1.,0.));
#10371=DIRECTION('center_axis',(0.,1.,0.));
#10372=DIRECTION('ref_axis',(1.,0.,0.));
#10373=DIRECTION('center_axis',(0.,-1.,0.));
#10374=DIRECTION('ref_axis',(1.,0.,0.));
#10375=DIRECTION('',(-0.707106781186548,0.707106781186547,-8.65956056235494E-17));
#10376=DIRECTION('center_axis',(0.,-1.,0.));
#10377=DIRECTION('ref_axis',(0.,0.,-1.));
#10378=DIRECTION('center_axis',(0.,-1.,0.));
#10379=DIRECTION('ref_axis',(1.,0.,0.));
#10380=DIRECTION('',(0.,1.,0.));
#10381=DIRECTION('axis',(0.,0.,1.));
#10382=DIRECTION('refdir',(1.,0.,0.));
#10383=DIRECTION('center_axis',(0.,0.,1.));
#10384=DIRECTION('ref_axis',(1.,0.,0.));
#10385=DIRECTION('center_axis',(1.22464679914735E-16,-1.,0.));
#10386=DIRECTION('ref_axis',(-1.,-1.22464679914735E-16,0.));
#10387=DIRECTION('center_axis',(0.707106781186548,0.,0.707106781186548));
#10388=DIRECTION('ref_axis',(0.707106781186548,0.,-0.707106781186548));
#10389=DIRECTION('center_axis',(8.65956056235494E-17,-1.,-8.65956056235493E-17));
#10390=DIRECTION('ref_axis',(-0.707106781186547,-1.22464679914735E-16,0.707106781186547));
#10391=DIRECTION('center_axis',(1.,0.,0.));
#10392=DIRECTION('ref_axis',(6.12323399573676E-17,0.,-1.));
#10393=DIRECTION('center_axis',(7.49879891330929E-33,-1.,-1.22464679914735E-16));
#10394=DIRECTION('ref_axis',(-6.12323399573676E-17,-1.22464679914735E-16,
1.));
#10395=DIRECTION('center_axis',(0.707106781186548,0.,-0.707106781186548));
#10396=DIRECTION('ref_axis',(-0.707106781186548,0.,-0.707106781186548));
#10397=DIRECTION('center_axis',(-8.65956056235493E-17,-1.,-8.65956056235494E-17));
#10398=DIRECTION('ref_axis',(0.707106781186547,-1.22464679914735E-16,0.707106781186547));
#10399=DIRECTION('center_axis',(0.,0.,-1.));
#10400=DIRECTION('ref_axis',(-1.,0.,-1.22464679914735E-16));
#10401=DIRECTION('center_axis',(-1.22464679914735E-16,-1.,-1.49975978266186E-32));
#10402=DIRECTION('ref_axis',(1.,-1.22464679914735E-16,1.22464679914735E-16));
#10403=DIRECTION('center_axis',(-0.707106781186547,0.,-0.707106781186548));
#10404=DIRECTION('ref_axis',(-0.707106781186548,0.,0.707106781186547));
#10405=DIRECTION('center_axis',(-8.65956056235493E-17,-1.,8.65956056235493E-17));
#10406=DIRECTION('ref_axis',(0.707106781186548,-1.22464679914735E-16,-0.707106781186547));
#10407=DIRECTION('center_axis',(-1.,0.,0.));
#10408=DIRECTION('ref_axis',(-1.83697019872103E-16,0.,1.));
#10409=DIRECTION('center_axis',(-2.24963967399279E-32,-1.,1.22464679914735E-16));
#10410=DIRECTION('ref_axis',(1.83697019872103E-16,-1.22464679914735E-16,
-1.));
#10411=DIRECTION('center_axis',(-0.707106781186548,0.,0.707106781186548));
#10412=DIRECTION('ref_axis',(0.707106781186547,0.,0.707106781186548));
#10413=DIRECTION('center_axis',(8.65956056235493E-17,-1.,8.65956056235493E-17));
#10414=DIRECTION('ref_axis',(-0.707106781186547,-1.22464679914735E-16,-0.707106781186548));
#10415=DIRECTION('axis',(0.,0.,1.));
#10416=DIRECTION('refdir',(1.,0.,0.));
#10417=DIRECTION('center_axis',(0.,0.,1.));
#10418=DIRECTION('ref_axis',(1.,0.,0.));
#10419=DIRECTION('center_axis',(0.,-1.,0.));
#10420=DIRECTION('ref_axis',(0.,0.,-1.));
#10421=DIRECTION('center_axis',(0.,-1.,0.));
#10422=DIRECTION('ref_axis',(0.,0.,-1.));
#10423=DIRECTION('center_axis',(0.,1.,0.));
#10424=DIRECTION('ref_axis',(1.,0.,0.));
#10425=DIRECTION('center_axis',(0.,1.,0.));
#10426=DIRECTION('ref_axis',(1.,0.,0.));
#10427=DIRECTION('center_axis',(0.,1.,0.));
#10428=DIRECTION('ref_axis',(1.,0.,0.));
#10429=DIRECTION('center_axis',(0.,1.,0.));
#10430=DIRECTION('ref_axis',(1.,0.,0.));
#10431=DIRECTION('',(0.,-1.,0.));
#10432=DIRECTION('center_axis',(0.,-1.,0.));
#10433=DIRECTION('ref_axis',(1.,0.,0.));
#10434=DIRECTION('center_axis',(0.,1.,0.));
#10435=DIRECTION('ref_axis',(1.,0.,0.));
#10436=DIRECTION('center_axis',(0.,1.,0.));
#10437=DIRECTION('ref_axis',(1.,0.,0.));
#10438=DIRECTION('center_axis',(0.,1.,0.));
#10439=DIRECTION('ref_axis',(1.,0.,0.));
#10440=DIRECTION('center_axis',(0.,1.,0.));
#10441=DIRECTION('ref_axis',(1.,0.,0.));
#10442=DIRECTION('center_axis',(0.,1.,0.));
#10443=DIRECTION('ref_axis',(1.,0.,0.));
#10444=DIRECTION('center_axis',(0.,1.,0.));
#10445=DIRECTION('ref_axis',(1.,0.,0.));
#10446=DIRECTION('center_axis',(0.,-1.,0.));
#10447=DIRECTION('ref_axis',(1.,0.,0.));
#10448=DIRECTION('center_axis',(0.,-1.,0.));
#10449=DIRECTION('ref_axis',(0.,0.,-1.));
#10450=DIRECTION('center_axis',(6.12323399573677E-17,0.,1.));
#10451=DIRECTION('ref_axis',(1.,0.,0.));
#10452=DIRECTION('center_axis',(0.,-1.,0.));
#10453=DIRECTION('ref_axis',(0.,0.,-1.));
#10454=DIRECTION('center_axis',(0.,1.,0.));
#10455=DIRECTION('ref_axis',(1.,0.,0.));
#10456=DIRECTION('center_axis',(0.,-1.,0.));
#10457=DIRECTION('ref_axis',(1.,0.,0.));
#10458=DIRECTION('center_axis',(0.,-1.,0.));
#10459=DIRECTION('ref_axis',(0.,0.,-1.));
#10460=DIRECTION('center_axis',(0.,0.,1.));
#10461=DIRECTION('ref_axis',(1.,0.,0.));
#10462=DIRECTION('center_axis',(0.,-1.,0.));
#10463=DIRECTION('ref_axis',(0.,0.,-1.));
#10464=DIRECTION('center_axis',(0.,1.,0.));
#10465=DIRECTION('ref_axis',(1.,0.,0.));
#10466=DIRECTION('center_axis',(0.,-1.,0.));
#10467=DIRECTION('ref_axis',(1.,0.,0.));
#10468=DIRECTION('center_axis',(0.,-1.,0.));
#10469=DIRECTION('ref_axis',(0.,0.,-1.));
#10470=DIRECTION('center_axis',(0.,0.,1.));
#10471=DIRECTION('ref_axis',(1.,0.,0.));
#10472=DIRECTION('center_axis',(0.,-1.,0.));
#10473=DIRECTION('ref_axis',(0.,0.,-1.));
#10474=DIRECTION('center_axis',(0.,1.,0.));
#10475=DIRECTION('ref_axis',(1.,0.,0.));
#10476=DIRECTION('center_axis',(0.,-1.,0.));
#10477=DIRECTION('ref_axis',(1.,0.,0.));
#10478=DIRECTION('center_axis',(0.,-1.,0.));
#10479=DIRECTION('ref_axis',(0.,0.,-1.));
#10480=DIRECTION('center_axis',(0.,0.,1.));
#10481=DIRECTION('ref_axis',(1.,0.,0.));
#10482=DIRECTION('center_axis',(0.,-1.,0.));
#10483=DIRECTION('ref_axis',(0.,0.,-1.));
#10484=DIRECTION('center_axis',(0.,1.,0.));
#10485=DIRECTION('ref_axis',(1.,0.,0.));
#10486=DIRECTION('center_axis',(0.,-1.,0.));
#10487=DIRECTION('ref_axis',(1.,0.,0.));
#10488=DIRECTION('center_axis',(0.,-1.,0.));
#10489=DIRECTION('ref_axis',(0.,0.,-1.));
#10490=DIRECTION('center_axis',(6.12323399573676E-17,0.,1.));
#10491=DIRECTION('ref_axis',(1.,0.,0.));
#10492=DIRECTION('center_axis',(0.,-1.,0.));
#10493=DIRECTION('ref_axis',(0.,0.,-1.));
#10494=DIRECTION('center_axis',(0.,1.,0.));
#10495=DIRECTION('ref_axis',(1.,0.,0.));
#10496=DIRECTION('center_axis',(0.,-1.,0.));
#10497=DIRECTION('ref_axis',(1.,0.,0.));
#10498=DIRECTION('center_axis',(0.,-1.,0.));
#10499=DIRECTION('ref_axis',(0.,0.,-1.));
#10500=DIRECTION('center_axis',(0.,0.,1.));
#10501=DIRECTION('ref_axis',(1.,0.,0.));
#10502=DIRECTION('center_axis',(0.,-1.,0.));
#10503=DIRECTION('ref_axis',(0.,0.,-1.));
#10504=DIRECTION('center_axis',(0.,1.,0.));
#10505=DIRECTION('ref_axis',(1.,0.,0.));
#10506=DIRECTION('center_axis',(0.,1.,0.));
#10507=DIRECTION('ref_axis',(1.,0.,0.));
#10508=DIRECTION('',(0.,1.,0.));
#10509=DIRECTION('center_axis',(0.,-1.,0.));
#10510=DIRECTION('ref_axis',(1.,0.,0.));
#10511=DIRECTION('center_axis',(0.,-1.,0.));
#10512=DIRECTION('ref_axis',(1.,0.,0.));
#10513=DIRECTION('center_axis',(0.,1.,0.));
#10514=DIRECTION('ref_axis',(1.,0.,0.));
#10515=DIRECTION('center_axis',(0.,-1.,0.));
#10516=DIRECTION('ref_axis',(0.,0.,-1.));
#10517=DIRECTION('center_axis',(0.,0.,1.));
#10518=DIRECTION('ref_axis',(1.,0.,0.));
#10519=DIRECTION('center_axis',(0.,-1.,0.));
#10520=DIRECTION('ref_axis',(0.,0.,-1.));
#10521=DIRECTION('center_axis',(0.,-1.,0.));
#10522=DIRECTION('ref_axis',(-1.,0.,0.));
#10523=DIRECTION('center_axis',(0.,1.,0.));
#10524=DIRECTION('ref_axis',(1.,0.,0.));
#10525=DIRECTION('axis',(0.,0.,1.));
#10526=DIRECTION('refdir',(1.,0.,0.));
#10527=DIRECTION('center_axis',(0.,1.,0.));
#10528=DIRECTION('ref_axis',(0.,0.,1.));
#10529=DIRECTION('center_axis',(0.,-1.,0.));
#10530=DIRECTION('ref_axis',(1.,0.,0.));
#10531=DIRECTION('center_axis',(0.,-1.,0.));
#10532=DIRECTION('ref_axis',(1.,0.,0.));
#10533=DIRECTION('center_axis',(0.,-1.,0.));
#10534=DIRECTION('ref_axis',(1.,0.,0.));
#10535=DIRECTION('center_axis',(0.,-1.,0.));
#10536=DIRECTION('ref_axis',(1.,0.,0.));
#10537=DIRECTION('',(0.,1.,0.));
#10538=DIRECTION('center_axis',(0.,-1.,0.));
#10539=DIRECTION('ref_axis',(0.,0.,-1.));
#10540=DIRECTION('center_axis',(0.,-1.,0.));
#10541=DIRECTION('ref_axis',(1.,0.,0.));
#10542=DIRECTION('center_axis',(0.,-1.,0.));
#10543=DIRECTION('ref_axis',(1.,0.,0.));
#10544=DIRECTION('',(0.,1.,0.));
#10545=DIRECTION('center_axis',(0.,1.,0.));
#10546=DIRECTION('ref_axis',(0.,0.,1.));
#10547=DIRECTION('center_axis',(0.,-1.,0.));
#10548=DIRECTION('ref_axis',(1.,0.,0.));
#10549=DIRECTION('center_axis',(0.,-1.,0.));
#10550=DIRECTION('ref_axis',(1.,0.,0.));
#10551=DIRECTION('center_axis',(0.,-1.,0.));
#10552=DIRECTION('ref_axis',(1.,0.,0.));
#10553=DIRECTION('center_axis',(0.,-1.,0.));
#10554=DIRECTION('ref_axis',(1.,0.,0.));
#10555=DIRECTION('',(0.,1.,0.));
#10556=DIRECTION('center_axis',(0.,-1.,0.));
#10557=DIRECTION('ref_axis',(0.,0.,-1.));
#10558=DIRECTION('center_axis',(0.,-1.,0.));
#10559=DIRECTION('ref_axis',(1.,0.,0.));
#10560=DIRECTION('center_axis',(0.,-1.,0.));
#10561=DIRECTION('ref_axis',(1.,0.,0.));
#10562=DIRECTION('',(0.,1.,0.));
#10563=DIRECTION('',(0.,0.,1.));
#10564=DIRECTION('',(1.,0.,0.));
#10565=DIRECTION('',(0.,0.,1.));
#10566=DIRECTION('',(1.,0.,0.));
#10567=DIRECTION('',(0.,0.,1.));
#10568=DIRECTION('',(1.,0.,0.));
#10569=DIRECTION('',(0.,0.,1.));
#10570=DIRECTION('',(1.,0.,0.));
#10571=DIRECTION('',(0.,0.,1.));
#10572=DIRECTION('',(1.,0.,0.));
#10573=DIRECTION('axis',(0.,0.,1.));
#10574=DIRECTION('refdir',(1.,0.,0.));
#10575=DIRECTION('center_axis',(0.,1.,0.));
#10576=DIRECTION('ref_axis',(1.,0.,0.));
#10577=DIRECTION('center_axis',(0.,-1.,0.));
#10578=DIRECTION('ref_axis',(1.,0.,0.));
#10579=DIRECTION('',(0.,-1.,0.));
#10580=DIRECTION('center_axis',(0.,-1.,0.));
#10581=DIRECTION('ref_axis',(1.,0.,0.));
#10582=DIRECTION('center_axis',(0.,1.,0.));
#10583=DIRECTION('ref_axis',(1.,0.,0.));
#10584=DIRECTION('center_axis',(0.,1.,0.));
#10585=DIRECTION('ref_axis',(1.,0.,0.));
#10586=DIRECTION('',(0.,-1.,0.));
#10587=DIRECTION('center_axis',(0.,1.,0.));
#10588=DIRECTION('ref_axis',(1.,0.,0.));
#10589=DIRECTION('center_axis',(0.,1.,0.));
#10590=DIRECTION('ref_axis',(1.,0.,0.));
#10591=DIRECTION('center_axis',(0.,1.,0.));
#10592=DIRECTION('ref_axis',(1.,0.,0.));
#10593=DIRECTION('axis',(0.,0.,1.));
#10594=DIRECTION('refdir',(1.,0.,0.));
#10595=DIRECTION('center_axis',(0.866025403784439,0.,-0.5));
#10596=DIRECTION('ref_axis',(0.5,0.,0.866025403784439));
#10597=DIRECTION('',(-0.5,0.,-0.866025403784439));
#10598=DIRECTION('',(0.,-1.,0.));
#10599=DIRECTION('',(0.5,0.,0.866025403784439));
#10600=DIRECTION('',(0.,-1.,0.));
#10601=DIRECTION('center_axis',(1.60246890531964E-16,0.,-1.));
#10602=DIRECTION('ref_axis',(1.,0.,1.60246890531964E-16));
#10603=DIRECTION('',(-1.,0.,-1.60246890531964E-16));
#10604=DIRECTION('',(0.,-1.,0.));
#10605=DIRECTION('',(1.,0.,1.60246890531964E-16));
#10606=DIRECTION('center_axis',(-0.866025403784439,0.,-0.5));
#10607=DIRECTION('ref_axis',(0.5,0.,-0.866025403784439));
#10608=DIRECTION('',(-0.5,0.,0.866025403784439));
#10609=DIRECTION('',(0.,-1.,0.));
#10610=DIRECTION('',(0.5,0.,-0.866025403784439));
#10611=DIRECTION('center_axis',(-0.866025403784439,0.,0.5));
#10612=DIRECTION('ref_axis',(-0.5,0.,-0.866025403784439));
#10613=DIRECTION('',(0.5,0.,0.866025403784439));
#10614=DIRECTION('',(0.,-1.,0.));
#10615=DIRECTION('',(-0.5,0.,-0.866025403784439));
#10616=DIRECTION('center_axis',(-1.60246890531964E-16,0.,1.));
#10617=DIRECTION('ref_axis',(-1.,0.,-1.60246890531964E-16));
#10618=DIRECTION('',(1.,0.,1.60246890531964E-16));
#10619=DIRECTION('',(0.,-1.,0.));
#10620=DIRECTION('',(-1.,0.,-1.60246890531964E-16));
#10621=DIRECTION('center_axis',(0.866025403784439,0.,0.5));
#10622=DIRECTION('ref_axis',(-0.5,0.,0.866025403784439));
#10623=DIRECTION('',(0.5,0.,-0.866025403784439));
#10624=DIRECTION('',(-0.5,0.,0.866025403784439));
#10625=DIRECTION('center_axis',(0.,1.,0.));
#10626=DIRECTION('ref_axis',(1.,0.,0.));
#10627=DIRECTION('center_axis',(0.,-1.,0.));
#10628=DIRECTION('ref_axis',(0.,0.,-1.));
#10629=DIRECTION('center_axis',(0.,1.,0.));
#10630=DIRECTION('ref_axis',(1.,0.,0.));
#10631=DIRECTION('center_axis',(0.,1.,0.));
#10632=DIRECTION('ref_axis',(1.,0.,0.));
#10633=DIRECTION('center_axis',(0.,1.,0.));
#10634=DIRECTION('ref_axis',(0.,0.,1.));
#10635=DIRECTION('center_axis',(0.,-1.,0.));
#10636=DIRECTION('ref_axis',(1.,0.,0.));
#10637=DIRECTION('center_axis',(0.,-1.,0.));
#10638=DIRECTION('ref_axis',(1.,0.,0.));
#10639=DIRECTION('center_axis',(0.,-1.,0.));
#10640=DIRECTION('ref_axis',(1.,0.,0.));
#10641=DIRECTION('',(0.707106781186547,0.707106781186548,8.65956056235493E-17));
#10642=DIRECTION('center_axis',(0.,-1.,0.));
#10643=DIRECTION('ref_axis',(1.,0.,0.));
#10644=DIRECTION('center_axis',(0.,-1.,0.));
#10645=DIRECTION('ref_axis',(1.,0.,0.));
#10646=DIRECTION('',(0.,1.,0.));
#10647=DIRECTION('center_axis',(0.,1.,0.));
#10648=DIRECTION('ref_axis',(1.,0.,0.));
#10649=DIRECTION('center_axis',(0.,-1.,0.));
#10650=DIRECTION('ref_axis',(1.,0.,0.));
#10651=DIRECTION('',(-0.707106781186547,0.707106781186548,-8.65956056235493E-17));
#10652=DIRECTION('center_axis',(0.,-1.,0.));
#10653=DIRECTION('ref_axis',(0.,0.,-1.));
#10654=DIRECTION('center_axis',(0.,-1.,0.));
#10655=DIRECTION('ref_axis',(1.,0.,0.));
#10656=DIRECTION('center_axis',(0.,1.,0.));
#10657=DIRECTION('ref_axis',(1.,0.,0.));
#10658=DIRECTION('center_axis',(0.,1.,0.));
#10659=DIRECTION('ref_axis',(1.,0.,0.));
#10660=DIRECTION('',(-0.447213595499958,0.894427190999916,-5.47678698264203E-17));
#10661=DIRECTION('center_axis',(0.,-1.,0.));
#10662=DIRECTION('ref_axis',(1.,0.,0.));
#10663=DIRECTION('',(0.,1.,0.));
#10664=DIRECTION('axis',(0.,0.,1.));
#10665=DIRECTION('refdir',(1.,0.,0.));
#10666=DIRECTION('center_axis',(0.,1.,0.));
#10667=DIRECTION('ref_axis',(1.,0.,0.));
#10668=DIRECTION('center_axis',(0.,-1.,0.));
#10669=DIRECTION('ref_axis',(1.,0.,0.));
#10670=DIRECTION('',(0.,-1.,0.));
#10671=DIRECTION('center_axis',(0.,-1.,0.));
#10672=DIRECTION('ref_axis',(1.,0.,0.));
#10673=DIRECTION('center_axis',(0.,1.,0.));
#10674=DIRECTION('ref_axis',(1.,0.,0.));
#10675=DIRECTION('center_axis',(0.,1.,0.));
#10676=DIRECTION('ref_axis',(1.,0.,0.));
#10677=DIRECTION('',(0.,-1.,0.));
#10678=DIRECTION('center_axis',(0.,1.,0.));
#10679=DIRECTION('ref_axis',(1.,0.,0.));
#10680=DIRECTION('center_axis',(0.,1.,0.));
#10681=DIRECTION('ref_axis',(1.,0.,0.));
#10682=DIRECTION('center_axis',(0.,1.,0.));
#10683=DIRECTION('ref_axis',(1.,0.,0.));
#10684=DIRECTION('axis',(0.,0.,1.));
#10685=DIRECTION('refdir',(1.,0.,0.));
#10686=DIRECTION('center_axis',(0.,0.,1.));
#10687=DIRECTION('ref_axis',(1.,0.,0.));
#10688=DIRECTION('',(1.,0.,0.));
#10689=DIRECTION('',(0.,-1.,0.));
#10690=DIRECTION('',(-1.,0.,0.));
#10691=DIRECTION('',(0.,1.,0.));
#10692=DIRECTION('center_axis',(0.,1.,0.));
#10693=DIRECTION('ref_axis',(-1.,0.,0.));
#10694=DIRECTION('',(0.,0.,1.));
#10695=DIRECTION('',(-1.,0.,0.));
#10696=DIRECTION('',(0.,0.,1.));
#10697=DIRECTION('center_axis',(0.,0.,1.));
#10698=DIRECTION('ref_axis',(1.,0.,0.));
#10699=DIRECTION('',(0.,-1.,0.));
#10700=DIRECTION('',(1.,0.,0.));
#10701=DIRECTION('',(0.,1.,0.));
#10702=DIRECTION('center_axis',(0.,0.,-1.));
#10703=DIRECTION('ref_axis',(1.,0.,0.));
#10704=DIRECTION('center_axis',(-1.,0.,0.));
#10705=DIRECTION('ref_axis',(0.,-1.,0.));
#10706=DIRECTION('',(0.,0.,1.));
#10707=DIRECTION('',(0.,0.707106781186548,0.707106781186548));
#10708=DIRECTION('',(0.,-1.,0.));
#10709=DIRECTION('',(0.,0.707106781186548,-0.707106781186548));
#10710=DIRECTION('',(0.,0.,1.));
#10711=DIRECTION('',(0.,-1.,0.));
#10712=DIRECTION('',(0.,0.,1.));
#10713=DIRECTION('center_axis',(0.,-1.,0.));
#10714=DIRECTION('ref_axis',(1.,0.,0.));
#10715=DIRECTION('',(1.,0.,0.));
#10716=DIRECTION('',(0.,0.,1.));
#10717=DIRECTION('center_axis',(0.,0.,1.));
#10718=DIRECTION('ref_axis',(1.,0.,0.));
#10719=DIRECTION('',(-1.,0.,0.));
#10720=DIRECTION('',(0.,1.,0.));
#10721=DIRECTION('center_axis',(1.,0.,0.));
#10722=DIRECTION('ref_axis',(0.,1.,0.));
#10723=DIRECTION('',(0.,0.,1.));
#10724=DIRECTION('',(0.,-0.707106781186548,0.707106781186548));
#10725=DIRECTION('',(0.,1.,0.));
#10726=DIRECTION('',(0.,-0.707106781186548,-0.707106781186548));
#10727=DIRECTION('',(0.,0.,1.));
#10728=DIRECTION('center_axis',(0.,-1.,0.));
#10729=DIRECTION('ref_axis',(1.,0.,0.));
#10730=DIRECTION('',(-1.,0.,0.));
#10731=DIRECTION('center_axis',(0.,-0.707106781186548,-0.707106781186548));
#10732=DIRECTION('ref_axis',(-1.,0.,0.));
#10733=DIRECTION('',(1.,0.,0.));
#10734=DIRECTION('center_axis',(0.,0.707106781186548,0.707106781186548));
#10735=DIRECTION('ref_axis',(0.,0.707106781186547,-0.707106781186547));
#10736=DIRECTION('',(1.,0.,0.));
#10737=DIRECTION('center_axis',(0.,0.,1.));
#10738=DIRECTION('ref_axis',(1.,0.,0.));
#10739=DIRECTION('center_axis',(0.,0.,-1.));
#10740=DIRECTION('ref_axis',(1.,0.,0.));
#10741=DIRECTION('',(0.,0.,1.));
#10742=DIRECTION('center_axis',(0.,0.,-1.));
#10743=DIRECTION('ref_axis',(1.,0.,0.));
#10744=DIRECTION('center_axis',(0.,-0.707106781186548,0.707106781186548));
#10745=DIRECTION('ref_axis',(0.,0.707106781186547,0.707106781186547));
#10746=DIRECTION('center_axis',(0.,0.,-1.));
#10747=DIRECTION('ref_axis',(1.,0.,0.));
#10748=DIRECTION('center_axis',(0.,0.,1.));
#10749=DIRECTION('ref_axis',(1.,0.,0.));
#10750=DIRECTION('',(-1.,0.,0.));
#10751=DIRECTION('center_axis',(0.,0.,1.));
#10752=DIRECTION('ref_axis',(1.,0.,0.));
#10753=DIRECTION('',(-1.,0.,0.));
#10754=DIRECTION('center_axis',(0.,0.707106781186548,-0.707106781186548));
#10755=DIRECTION('ref_axis',(-1.,0.,0.));
#10756=DIRECTION('',(1.,0.,0.));
#10757=DIRECTION('center_axis',(0.,1.,0.));
#10758=DIRECTION('ref_axis',(-1.,0.,0.));
#10759=DIRECTION('axis',(0.,0.,1.));
#10760=DIRECTION('refdir',(1.,0.,0.));
#10761=DIRECTION('center_axis',(0.866025403784439,0.,-0.5));
#10762=DIRECTION('ref_axis',(0.5,0.,0.866025403784439));
#10763=DIRECTION('',(-0.5,0.,-0.866025403784439));
#10764=DIRECTION('',(0.,-1.,0.));
#10765=DIRECTION('',(0.5,0.,0.866025403784439));
#10766=DIRECTION('',(0.,-1.,0.));
#10767=DIRECTION('center_axis',(1.20185167898973E-16,0.,-1.));
#10768=DIRECTION('ref_axis',(1.,0.,1.20185167898973E-16));
#10769=DIRECTION('',(-1.,0.,-1.20185167898973E-16));
#10770=DIRECTION('',(0.,-1.,0.));
#10771=DIRECTION('',(1.,0.,1.20185167898973E-16));
#10772=DIRECTION('center_axis',(-0.866025403784439,0.,-0.5));
#10773=DIRECTION('ref_axis',(0.5,0.,-0.866025403784439));
#10774=DIRECTION('',(-0.5,0.,0.866025403784439));
#10775=DIRECTION('',(0.,-1.,0.));
#10776=DIRECTION('',(0.5,0.,-0.866025403784439));
#10777=DIRECTION('center_axis',(-0.866025403784439,0.,0.5));
#10778=DIRECTION('ref_axis',(-0.5,0.,-0.866025403784439));
#10779=DIRECTION('',(0.5,0.,0.866025403784439));
#10780=DIRECTION('',(0.,-1.,0.));
#10781=DIRECTION('',(-0.5,0.,-0.866025403784439));
#10782=DIRECTION('center_axis',(-2.40370335797945E-16,0.,1.));
#10783=DIRECTION('ref_axis',(-1.,0.,-2.40370335797945E-16));
#10784=DIRECTION('',(1.,0.,2.40370335797945E-16));
#10785=DIRECTION('',(0.,-1.,0.));
#10786=DIRECTION('',(-1.,0.,-2.40370335797945E-16));
#10787=DIRECTION('center_axis',(0.866025403784439,0.,0.5));
#10788=DIRECTION('ref_axis',(-0.5,0.,0.866025403784439));
#10789=DIRECTION('',(0.5,0.,-0.866025403784439));
#10790=DIRECTION('',(-0.5,0.,0.866025403784439));
#10791=DIRECTION('center_axis',(0.,1.,0.));
#10792=DIRECTION('ref_axis',(1.,0.,0.));
#10793=DIRECTION('center_axis',(0.,-1.,0.));
#10794=DIRECTION('ref_axis',(0.,0.,-1.));
#10795=DIRECTION('center_axis',(0.,1.,0.));
#10796=DIRECTION('ref_axis',(1.,0.,0.));
#10797=DIRECTION('center_axis',(0.,1.,0.));
#10798=DIRECTION('ref_axis',(1.,0.,0.));
#10799=DIRECTION('center_axis',(0.,1.,0.));
#10800=DIRECTION('ref_axis',(0.,0.,1.));
#10801=DIRECTION('center_axis',(0.,-1.,0.));
#10802=DIRECTION('ref_axis',(1.,0.,0.));
#10803=DIRECTION('center_axis',(0.,-1.,0.));
#10804=DIRECTION('ref_axis',(1.,0.,0.));
#10805=DIRECTION('center_axis',(0.,-1.,0.));
#10806=DIRECTION('ref_axis',(1.,0.,0.));
#10807=DIRECTION('',(0.707106781186548,0.707106781186547,8.65956056235493E-17));
#10808=DIRECTION('center_axis',(0.,-1.,0.));
#10809=DIRECTION('ref_axis',(1.,0.,0.));
#10810=DIRECTION('center_axis',(0.,-1.,0.));
#10811=DIRECTION('ref_axis',(1.,0.,0.));
#10812=DIRECTION('',(0.,1.,0.));
#10813=DIRECTION('center_axis',(0.,1.,0.));
#10814=DIRECTION('ref_axis',(1.,0.,0.));
#10815=DIRECTION('center_axis',(0.,-1.,0.));
#10816=DIRECTION('ref_axis',(1.,0.,0.));
#10817=DIRECTION('',(-0.707106781186547,0.707106781186548,-8.65956056235493E-17));
#10818=DIRECTION('center_axis',(0.,-1.,0.));
#10819=DIRECTION('ref_axis',(0.,0.,-1.));
#10820=DIRECTION('center_axis',(0.,-1.,0.));
#10821=DIRECTION('ref_axis',(1.,0.,0.));
#10822=DIRECTION('center_axis',(0.,1.,0.));
#10823=DIRECTION('ref_axis',(1.,0.,0.));
#10824=DIRECTION('center_axis',(0.,1.,0.));
#10825=DIRECTION('ref_axis',(1.,0.,0.));
#10826=DIRECTION('',(-0.447213595499958,0.894427190999916,-5.47678698264203E-17));
#10827=DIRECTION('center_axis',(0.,-1.,0.));
#10828=DIRECTION('ref_axis',(1.,0.,0.));
#10829=DIRECTION('',(0.,1.,0.));
#10830=DIRECTION('',(0.,0.,1.));
#10831=DIRECTION('',(1.,0.,0.));
#10832=DIRECTION('',(0.,0.,1.));
#10833=DIRECTION('',(1.,0.,0.));
#10834=DIRECTION('',(-1.,0.,2.22044604925031E-16));
#10835=DIRECTION('',(2.22044604925031E-16,0.,1.));
#10836=DIRECTION('',(0.,-1.,2.22044604925031E-16));
#10837=DIRECTION('',(1.,0.,0.));
#10838=DIRECTION('',(0.,-1.,2.22044604925031E-16));
#10839=DIRECTION('',(1.,0.,0.));
#10840=DIRECTION('',(0.,1.,2.22044604925031E-16));
#10841=DIRECTION('',(1.,0.,0.));
#10842=DIRECTION('',(0.,1.,2.22044604925031E-16));
#10843=DIRECTION('',(1.,0.,0.));
#10844=DIRECTION('',(-1.,0.,2.22044604925031E-16));
#10845=DIRECTION('',(2.22044604925031E-16,0.,1.));
#10846=DIRECTION('',(0.,-1.,2.22044604925031E-16));
#10847=DIRECTION('',(1.,0.,0.));
#10848=DIRECTION('',(0.,-1.,2.22044604925031E-16));
#10849=DIRECTION('',(1.,0.,0.));
#10850=DIRECTION('',(0.,1.,2.22044604925031E-16));
#10851=DIRECTION('',(1.,0.,0.));
#10852=DIRECTION('',(0.,1.,2.22044604925031E-16));
#10853=DIRECTION('',(1.,0.,0.));
#10854=DIRECTION('',(0.,0.,1.));
#10855=DIRECTION('',(1.,0.,0.));
#10856=DIRECTION('',(0.,-1.,0.));
#10857=DIRECTION('',(1.,0.,0.));
#10858=DIRECTION('',(0.,0.,1.));
#10859=DIRECTION('',(-1.,1.22464679914735E-16,0.));
#10860=DIRECTION('',(0.,0.,1.));
#10861=DIRECTION('',(-1.,1.22464679914735E-16,0.));
#10862=DIRECTION('',(0.,-1.,0.));
#10863=DIRECTION('',(1.,0.,0.));
#10864=DIRECTION('',(0.,0.,1.));
#10865=DIRECTION('',(-1.,1.22464679914735E-16,0.));
#10866=DIRECTION('',(0.,0.,1.));
#10867=DIRECTION('',(-1.,1.22464679914735E-16,0.));
#10868=DIRECTION('',(0.,-1.,0.));
#10869=DIRECTION('',(1.,0.,0.));
#10870=DIRECTION('',(0.,0.,1.));
#10871=DIRECTION('',(-1.,1.22464679914735E-16,0.));
#10872=DIRECTION('',(0.,0.,1.));
#10873=DIRECTION('',(-1.,1.22464679914735E-16,0.));
#10874=DIRECTION('',(0.,-1.,0.));
#10875=DIRECTION('',(1.,0.,0.));
#10876=DIRECTION('',(0.,0.,1.));
#10877=DIRECTION('',(-1.,1.22464679914735E-16,0.));
#10878=DIRECTION('',(0.,0.,1.));
#10879=DIRECTION('',(-1.,1.22464679914735E-16,0.));
#10880=DIRECTION('',(0.,0.,1.));
#10881=DIRECTION('',(1.,0.,0.));
#10882=DIRECTION('',(0.,0.,1.));
#10883=DIRECTION('',(1.,0.,0.));
#10884=DIRECTION('',(-1.,0.,2.22044604925031E-16));
#10885=DIRECTION('',(2.22044604925031E-16,0.,1.));
#10886=DIRECTION('',(0.,-1.,2.22044604925031E-16));
#10887=DIRECTION('',(1.,0.,0.));
#10888=DIRECTION('',(0.,-1.,2.22044604925031E-16));
#10889=DIRECTION('',(1.,0.,0.));
#10890=DIRECTION('',(0.,1.,2.22044604925031E-16));
#10891=DIRECTION('',(1.,0.,0.));
#10892=DIRECTION('',(0.,1.,2.22044604925031E-16));
#10893=DIRECTION('',(1.,0.,0.));
#10894=DIRECTION('',(-1.,0.,2.22044604925031E-16));
#10895=DIRECTION('',(2.22044604925031E-16,0.,1.));
#10896=DIRECTION('',(0.,-1.,2.22044604925031E-16));
#10897=DIRECTION('',(1.,0.,0.));
#10898=DIRECTION('',(0.,-1.,2.22044604925031E-16));
#10899=DIRECTION('',(1.,0.,0.));
#10900=DIRECTION('',(0.,1.,2.22044604925031E-16));
#10901=DIRECTION('',(1.,0.,0.));
#10902=DIRECTION('',(0.,1.,2.22044604925031E-16));
#10903=DIRECTION('',(1.,0.,0.));
#10904=DIRECTION('',(0.,0.,1.));
#10905=DIRECTION('',(1.,0.,0.));
#10906=DIRECTION('',(0.,1.,0.));
#10907=DIRECTION('',(1.,0.,0.));
#10908=DIRECTION('',(0.,0.,1.));
#10909=DIRECTION('',(1.,0.,0.));
#10910=DIRECTION('',(0.,0.,1.));
#10911=DIRECTION('',(1.,0.,0.));
#10912=DIRECTION('',(0.,1.,0.));
#10913=DIRECTION('',(1.,0.,0.));
#10914=DIRECTION('',(0.,0.,1.));
#10915=DIRECTION('',(1.,0.,0.));
#10916=DIRECTION('',(0.,0.,1.));
#10917=DIRECTION('',(1.,0.,0.));
#10918=DIRECTION('',(0.,1.,0.));
#10919=DIRECTION('',(1.,0.,0.));
#10920=DIRECTION('',(0.,0.,1.));
#10921=DIRECTION('',(1.,0.,0.));
#10922=DIRECTION('',(0.,0.,1.));
#10923=DIRECTION('',(1.,0.,0.));
#10924=DIRECTION('',(0.,1.,0.));
#10925=DIRECTION('',(1.,0.,0.));
#10926=DIRECTION('',(0.,0.,1.));
#10927=DIRECTION('',(1.,0.,0.));
#10928=DIRECTION('',(0.,0.,1.));
#10929=DIRECTION('',(1.,0.,0.));
#10930=DIRECTION('',(0.,0.,1.));
#10931=DIRECTION('',(1.,0.,0.));
#10932=DIRECTION('',(0.,0.,1.));
#10933=DIRECTION('',(1.,0.,0.));
#10934=DIRECTION('',(0.,0.,1.));
#10935=DIRECTION('',(1.,0.,0.));
#10936=DIRECTION('',(0.,0.,1.));
#10937=DIRECTION('',(1.,0.,0.));
#10938=DIRECTION('',(0.,0.,1.));
#10939=DIRECTION('',(1.,0.,0.));
#10940=DIRECTION('',(0.,0.,1.));
#10941=DIRECTION('',(1.,0.,0.));
#10942=DIRECTION('axis',(0.,0.,1.));
#10943=DIRECTION('refdir',(1.,0.,0.));
#10944=DIRECTION('center_axis',(0.,0.,1.));
#10945=DIRECTION('ref_axis',(1.,0.,0.));
#10946=DIRECTION('center_axis',(0.,0.,1.));
#10947=DIRECTION('ref_axis',(1.,0.,0.));
#10948=DIRECTION('',(0.,0.,1.));
#10949=DIRECTION('center_axis',(0.,0.,-1.));
#10950=DIRECTION('ref_axis',(1.,0.,0.));
#10951=DIRECTION('center_axis',(0.,0.,1.));
#10952=DIRECTION('ref_axis',(1.,0.,0.));
#10953=DIRECTION('center_axis',(0.,0.,1.));
#10954=DIRECTION('ref_axis',(1.,0.,0.));
#10955=DIRECTION('center_axis',(0.,0.,1.));
#10956=DIRECTION('ref_axis',(1.,0.,0.));
#10957=DIRECTION('center_axis',(0.,0.,1.));
#10958=DIRECTION('ref_axis',(1.,0.,0.));
#10959=DIRECTION('',(0.,0.,1.));
#10960=DIRECTION('center_axis',(0.,0.,-1.));
#10961=DIRECTION('ref_axis',(1.,0.,0.));
#10962=DIRECTION('center_axis',(0.,0.,1.));
#10963=DIRECTION('ref_axis',(1.,0.,0.));
#10964=DIRECTION('center_axis',(0.,0.,1.));
#10965=DIRECTION('ref_axis',(1.,0.,0.));
#10966=DIRECTION('center_axis',(0.,0.,1.));
#10967=DIRECTION('ref_axis',(1.,0.,0.));
#10968=DIRECTION('center_axis',(0.,0.,1.));
#10969=DIRECTION('ref_axis',(1.,0.,0.));
#10970=DIRECTION('',(0.,0.,1.));
#10971=DIRECTION('center_axis',(0.,0.,1.));
#10972=DIRECTION('ref_axis',(1.,0.,0.));
#10973=DIRECTION('center_axis',(0.,0.,1.));
#10974=DIRECTION('ref_axis',(1.,0.,0.));
#10975=DIRECTION('',(0.,0.,1.));
#10976=DIRECTION('center_axis',(0.,1.,0.));
#10977=DIRECTION('ref_axis',(1.,0.,0.));
#10978=DIRECTION('center_axis',(0.,1.,0.));
#10979=DIRECTION('ref_axis',(1.,0.,0.));
#10980=DIRECTION('',(0.,1.,0.));
#10981=DIRECTION('center_axis',(0.,-1.,0.));
#10982=DIRECTION('ref_axis',(1.,0.,0.));
#10983=DIRECTION('center_axis',(0.,1.,0.));
#10984=DIRECTION('ref_axis',(-1.,0.,0.));
#10985=DIRECTION('',(-1.,0.,0.));
#10986=DIRECTION('',(0.,0.,1.));
#10987=DIRECTION('',(-1.,0.,0.));
#10988=DIRECTION('',(0.,0.,1.));
#10989=DIRECTION('center_axis',(1.,0.,0.));
#10990=DIRECTION('ref_axis',(0.,1.,0.));
#10991=DIRECTION('',(0.,1.,0.));
#10992=DIRECTION('',(0.,1.,0.));
#10993=DIRECTION('',(0.,0.,1.));
#10994=DIRECTION('center_axis',(0.,-1.,0.));
#10995=DIRECTION('ref_axis',(1.,0.,0.));
#10996=DIRECTION('',(1.,0.,0.));
#10997=DIRECTION('',(1.,0.,0.));
#10998=DIRECTION('',(0.,0.,1.));
#10999=DIRECTION('center_axis',(-1.,0.,0.));
#11000=DIRECTION('ref_axis',(0.,-1.,0.));
#11001=DIRECTION('',(0.,-1.,0.));
#11002=DIRECTION('',(0.,-1.,0.));
#11003=DIRECTION('center_axis',(0.,0.,1.));
#11004=DIRECTION('ref_axis',(1.,0.,0.));
#11005=DIRECTION('center_axis',(0.,0.,1.));
#11006=DIRECTION('ref_axis',(1.,0.,0.));
#11007=DIRECTION('',(0.,0.,1.));
#11008=DIRECTION('',(1.,0.,0.));
#11009=DIRECTION('',(0.,0.,1.));
#11010=DIRECTION('',(1.,0.,0.));
#11011=DIRECTION('',(0.,0.,1.));
#11012=DIRECTION('',(1.,0.,0.));
#11013=DIRECTION('',(0.,0.,1.));
#11014=DIRECTION('',(1.,0.,0.));
#11015=DIRECTION('',(0.,0.,1.));
#11016=DIRECTION('',(1.,0.,0.));
#11017=DIRECTION('',(0.,0.,1.));
#11018=DIRECTION('',(1.,0.,0.));
#11019=DIRECTION('',(0.,0.,1.));
#11020=DIRECTION('',(1.,0.,0.));
#11021=DIRECTION('',(0.,0.,1.));
#11022=DIRECTION('',(1.,0.,0.));
#11023=DIRECTION('',(0.,0.,1.));
#11024=DIRECTION('',(1.,0.,0.));
#11025=DIRECTION('',(0.,0.,1.));
#11026=DIRECTION('',(1.,0.,0.));
#11027=DIRECTION('',(0.,0.,1.));
#11028=DIRECTION('',(-1.,1.22464679914735E-16,0.));
#11029=DIRECTION('',(0.,0.,1.));
#11030=DIRECTION('',(1.,0.,0.));
#11031=DIRECTION('',(0.,-1.,2.22044604925031E-16));
#11032=DIRECTION('',(1.,0.,0.));
#11033=DIRECTION('',(0.,-1.,2.22044604925031E-16));
#11034=DIRECTION('',(1.,0.,0.));
#11035=DIRECTION('',(0.,0.,1.));
#11036=DIRECTION('',(1.,0.,0.));
#11037=DIRECTION('',(0.,0.,1.));
#11038=DIRECTION('',(1.,0.,0.));
#11039=DIRECTION('',(0.,0.,1.));
#11040=DIRECTION('',(1.,0.,0.));
#11041=DIRECTION('',(0.,0.,1.));
#11042=DIRECTION('',(1.,0.,0.));
#11043=DIRECTION('',(0.,0.,1.));
#11044=DIRECTION('',(1.,0.,0.));
#11045=DIRECTION('',(0.,0.,1.));
#11046=DIRECTION('',(1.,0.,0.));
#11047=DIRECTION('',(0.,-1.,2.22044604925031E-16));
#11048=DIRECTION('',(1.,0.,0.));
#11049=DIRECTION('',(0.,0.,1.));
#11050=DIRECTION('',(1.,0.,0.));
#11051=DIRECTION('',(0.,-1.,2.22044604925031E-16));
#11052=DIRECTION('',(1.,0.,0.));
#11053=DIRECTION('',(0.,0.,1.));
#11054=DIRECTION('',(1.,0.,0.));
#11055=DIRECTION('',(0.,0.,1.));
#11056=DIRECTION('',(1.,0.,0.));
#11057=DIRECTION('',(0.,0.,1.));
#11058=DIRECTION('',(1.,0.,0.));
#11059=DIRECTION('',(0.,0.,1.));
#11060=DIRECTION('',(1.,0.,0.));
#11061=DIRECTION('',(0.,0.,1.));
#11062=DIRECTION('',(1.,0.,0.));
#11063=DIRECTION('',(0.,0.,1.));
#11064=DIRECTION('',(1.,0.,0.));
#11065=DIRECTION('',(0.,0.,1.));
#11066=DIRECTION('',(1.,0.,0.));
#11067=DIRECTION('',(0.,0.,1.));
#11068=DIRECTION('',(1.,0.,0.));
#11069=DIRECTION('',(0.,0.,1.));
#11070=DIRECTION('',(1.,0.,0.));
#11071=DIRECTION('',(0.,0.,1.));
#11072=DIRECTION('',(1.,0.,0.));
#11073=CARTESIAN_POINT('',(0.,0.,0.));
#11074=CARTESIAN_POINT('',(0.,0.,0.));
#11075=CARTESIAN_POINT('',(0.,0.,0.));
#11076=CARTESIAN_POINT('Origin',(42.,-3.9,5.));
#11077=CARTESIAN_POINT('',(41.725,-3.8,5.));
#11078=CARTESIAN_POINT('Origin',(42.,-3.8,5.));
#11079=CARTESIAN_POINT('',(41.725,-3.,5.));
#11080=CARTESIAN_POINT('',(41.725,-3.9,5.));
#11081=CARTESIAN_POINT('Origin',(42.,-3.,5.));
#11082=CARTESIAN_POINT('Origin',(39.,-3.9,5.));
#11083=CARTESIAN_POINT('',(38.725,-3.8,5.));
#11084=CARTESIAN_POINT('Origin',(39.,-3.8,5.));
#11085=CARTESIAN_POINT('',(38.725,-3.,5.));
#11086=CARTESIAN_POINT('',(38.725,-3.9,5.));
#11087=CARTESIAN_POINT('Origin',(39.,-3.,5.));
#11088=CARTESIAN_POINT('Origin',(36.,-3.9,5.));
#11089=CARTESIAN_POINT('',(35.725,-3.8,5.));
#11090=CARTESIAN_POINT('Origin',(36.,-3.8,5.));
#11091=CARTESIAN_POINT('',(35.725,-3.,5.));
#11092=CARTESIAN_POINT('',(35.725,-3.9,5.));
#11093=CARTESIAN_POINT('Origin',(36.,-3.,5.));
#11094=CARTESIAN_POINT('Origin',(45.,-3.9,5.));
#11095=CARTESIAN_POINT('',(44.725,-3.8,5.));
#11096=CARTESIAN_POINT('Origin',(45.,-3.8,5.));
#11097=CARTESIAN_POINT('',(44.725,-3.,5.));
#11098=CARTESIAN_POINT('',(44.725,-3.9,5.));
#11099=CARTESIAN_POINT('Origin',(45.,-3.,5.));
#11100=CARTESIAN_POINT('Origin',(46.,-3.,4.));
#11101=CARTESIAN_POINT('',(46.,-3.,4.));
#11102=CARTESIAN_POINT('',(35.,-3.,4.));
#11103=CARTESIAN_POINT('',(46.,-3.,4.));
#11104=CARTESIAN_POINT('',(35.,-3.,6.));
#11105=CARTESIAN_POINT('',(35.,-3.,4.));
#11106=CARTESIAN_POINT('',(46.,-3.,6.));
#11107=CARTESIAN_POINT('',(46.,-3.,6.));
#11108=CARTESIAN_POINT('',(46.,-3.,4.));
#11109=CARTESIAN_POINT('Origin',(46.,-3.8,4.));
#11110=CARTESIAN_POINT('',(46.,-3.8,4.));
#11111=CARTESIAN_POINT('',(46.,-3.8,4.));
#11112=CARTESIAN_POINT('',(46.,-3.8,6.));
#11113=CARTESIAN_POINT('',(46.,-3.8,6.));
#11114=CARTESIAN_POINT('',(46.,-3.8,4.));
#11115=CARTESIAN_POINT('Origin',(35.,-3.8,4.));
#11116=CARTESIAN_POINT('',(35.,-3.8,4.));
#11117=CARTESIAN_POINT('',(35.,-3.8,4.));
#11118=CARTESIAN_POINT('',(35.,-3.8,6.));
#11119=CARTESIAN_POINT('',(35.,-3.8,6.));
#11120=CARTESIAN_POINT('',(35.,-3.8,4.));
#11121=CARTESIAN_POINT('Origin',(35.,-3.,4.));
#11122=CARTESIAN_POINT('',(35.,-3.,4.));
#11123=CARTESIAN_POINT('',(35.,-3.,6.));
#11124=CARTESIAN_POINT('Origin',(40.5,-3.4,6.));
#11125=CARTESIAN_POINT('Origin',(40.5,-3.4,4.));
#11126=CARTESIAN_POINT('',(0.,0.,0.));
#11127=CARTESIAN_POINT('Origin',(6.,0.,-1.1));
#11128=CARTESIAN_POINT('',(5.725,-3.36777869765523E-17,-0.42));
#11129=CARTESIAN_POINT('Origin',(6.,0.,-0.42));
#11130=CARTESIAN_POINT('',(5.725,-4.4594469103905E-17,-0.21));
#11131=CARTESIAN_POINT('',(5.725,-3.36777869765523E-17,-1.1));
#11132=CARTESIAN_POINT('',(5.725,3.97778822344556E-18,0.21));
#11133=CARTESIAN_POINT('Ctrl Pts',(5.725,3.81639164714898E-17,0.21));
#11134=CARTESIAN_POINT('Ctrl Pts',(5.725,-0.027663639322611,0.21));
#11135=CARTESIAN_POINT('Ctrl Pts',(5.72949374752355,-0.0563806217319961,
0.204214038345313));
#11136=CARTESIAN_POINT('Ctrl Pts',(5.74560158587233,-0.107860332287473,
0.182341144032028));
#11137=CARTESIAN_POINT('Ctrl Pts',(5.75710894103549,-0.130678518444188,
0.166306329654162));
#11138=CARTESIAN_POINT('Ctrl Pts',(5.78023922617715,-0.166732877511574,
0.130251970586776));
#11139=CARTESIAN_POINT('Ctrl Pts',(5.7937414503193,-0.182517999394844,0.107475484252794));
#11140=CARTESIAN_POINT('Ctrl Pts',(5.80974723471181,-0.198712082533353,
0.0693141634661022));
#11141=CARTESIAN_POINT('Ctrl Pts',(5.81433611385285,-0.202908887997328,
0.0559106681449083));
#11142=CARTESIAN_POINT('Ctrl Pts',(5.82070090566933,-0.208554382393535,
0.0283388251429182));
#11143=CARTESIAN_POINT('Ctrl Pts',(5.82244719095435,-0.21,0.0141630178371274));
#11144=CARTESIAN_POINT('Ctrl Pts',(5.82244719095435,-0.21,-0.0141630178371274));
#11145=CARTESIAN_POINT('Ctrl Pts',(5.82070090566933,-0.208554382393535,
-0.0283388251429182));
#11146=CARTESIAN_POINT('Ctrl Pts',(5.81433611385285,-0.202908887997328,
-0.0559106681449083));
#11147=CARTESIAN_POINT('Ctrl Pts',(5.80974723471181,-0.198712082533353,
-0.0693141634661022));
#11148=CARTESIAN_POINT('Ctrl Pts',(5.7937414503193,-0.182517999394844,-0.107475484252795));
#11149=CARTESIAN_POINT('Ctrl Pts',(5.78023922617715,-0.166732877511574,
-0.130251970586776));
#11150=CARTESIAN_POINT('Ctrl Pts',(5.75710894103549,-0.130678518444188,
-0.166306329654162));
#11151=CARTESIAN_POINT('Ctrl Pts',(5.74560158587233,-0.107860332287473,
-0.182341144032028));
#11152=CARTESIAN_POINT('Ctrl Pts',(5.72949374752355,-0.0563806217319961,
-0.204214038345313));
#11153=CARTESIAN_POINT('Ctrl Pts',(5.725,-0.0276636393226111,-0.21));
#11154=CARTESIAN_POINT('Ctrl Pts',(5.725,-5.55111512312578E-17,-0.21));
#11155=CARTESIAN_POINT('',(5.725,3.36777869765523E-17,0.42));
#11156=CARTESIAN_POINT('',(5.725,-3.36777869765523E-17,-1.1));
#11157=CARTESIAN_POINT('Origin',(6.,0.,0.42));
#11158=CARTESIAN_POINT('',(5.82244719095435,0.21,2.25514051876985E-17));
#11159=CARTESIAN_POINT('Ctrl Pts',(5.82244719095435,0.21,2.25514051876985E-17));
#11160=CARTESIAN_POINT('Ctrl Pts',(5.82244719095435,0.21,0.0141630178371274));
#11161=CARTESIAN_POINT('Ctrl Pts',(5.82070090566933,0.208554382393535,0.0283388251429182));
#11162=CARTESIAN_POINT('Ctrl Pts',(5.81433611385285,0.202908887997328,0.0559106681449083));
#11163=CARTESIAN_POINT('Ctrl Pts',(5.80974723471181,0.198712082533353,0.0693141634661021));
#11164=CARTESIAN_POINT('Ctrl Pts',(5.7937414503193,0.182517999394844,0.107475484252794));
#11165=CARTESIAN_POINT('Ctrl Pts',(5.78023922617715,0.166732877511574,0.130251970586776));
#11166=CARTESIAN_POINT('Ctrl Pts',(5.75710894103549,0.130678518444188,0.166306329654162));
#11167=CARTESIAN_POINT('Ctrl Pts',(5.74560158587233,0.107860332287473,0.182341144032028));
#11168=CARTESIAN_POINT('Ctrl Pts',(5.72949374752355,0.0563806217319962,
0.204214038345313));
#11169=CARTESIAN_POINT('Ctrl Pts',(5.725,0.027663639322611,0.21));
#11170=CARTESIAN_POINT('Ctrl Pts',(5.725,6.93889390390723E-18,0.21));
#11171=CARTESIAN_POINT('Ctrl Pts',(5.725,-5.89805981832114E-17,-0.21));
#11172=CARTESIAN_POINT('Ctrl Pts',(5.725,0.0276636393226109,-0.21));
#11173=CARTESIAN_POINT('Ctrl Pts',(5.72949374752355,0.056380621731996,-0.204214038345314));
#11174=CARTESIAN_POINT('Ctrl Pts',(5.74560158587233,0.107860332287473,-0.182341144032028));
#11175=CARTESIAN_POINT('Ctrl Pts',(5.75710894103549,0.130678518444188,-0.166306329654162));
#11176=CARTESIAN_POINT('Ctrl Pts',(5.78023922617715,0.166732877511574,-0.130251970586776));
#11177=CARTESIAN_POINT('Ctrl Pts',(5.7937414503193,0.182517999394844,-0.107475484252795));
#11178=CARTESIAN_POINT('Ctrl Pts',(5.80974723471181,0.198712082533353,-0.0693141634661021));
#11179=CARTESIAN_POINT('Ctrl Pts',(5.81433611385285,0.202908887997328,-0.0559106681449082));
#11180=CARTESIAN_POINT('Ctrl Pts',(5.82070090566933,0.208554382393535,-0.0283388251429182));
#11181=CARTESIAN_POINT('Ctrl Pts',(5.82244719095435,0.21,-0.0141630178371274));
#11182=CARTESIAN_POINT('Ctrl Pts',(5.82244719095435,0.21,-6.24500451351651E-17));
#11183=CARTESIAN_POINT('',(6.17755280904565,0.21,3.29597460435593E-17));
#11184=CARTESIAN_POINT('',(6.275,4.48844336872086E-18,0.21));
#11185=CARTESIAN_POINT('Ctrl Pts',(6.17755280904565,0.21,3.29597460435593E-17));
#11186=CARTESIAN_POINT('Ctrl Pts',(6.17755280904565,0.21,-0.0141630178371274));
#11187=CARTESIAN_POINT('Ctrl Pts',(6.17929909433067,0.208554382393535,-0.0283388251429182));
#11188=CARTESIAN_POINT('Ctrl Pts',(6.18566388614715,0.202908887997328,-0.0559106681449083));
#11189=CARTESIAN_POINT('Ctrl Pts',(6.19025276528819,0.198712082533353,-0.0693141634661022));
#11190=CARTESIAN_POINT('Ctrl Pts',(6.2062585496807,0.182517999394844,-0.107475484252795));
#11191=CARTESIAN_POINT('Ctrl Pts',(6.21976077382285,0.166732877511574,-0.130251970586776));
#11192=CARTESIAN_POINT('Ctrl Pts',(6.24289105896451,0.130678518444188,-0.166306329654162));
#11193=CARTESIAN_POINT('Ctrl Pts',(6.25439841412767,0.107860332287473,-0.182341144032028));
#11194=CARTESIAN_POINT('Ctrl Pts',(6.27050625247645,0.056380621731996,-0.204214038345313));
#11195=CARTESIAN_POINT('Ctrl Pts',(6.275,0.027663639322611,-0.21));
#11196=CARTESIAN_POINT('Ctrl Pts',(6.275,-0.027663639322611,-0.21));
#11197=CARTESIAN_POINT('Ctrl Pts',(6.27050625247645,-0.0563806217319961,
-0.204214038345313));
#11198=CARTESIAN_POINT('Ctrl Pts',(6.25439841412767,-0.107860332287473,
-0.182341144032028));
#11199=CARTESIAN_POINT('Ctrl Pts',(6.24289105896451,-0.130678518444188,
-0.166306329654162));
#11200=CARTESIAN_POINT('Ctrl Pts',(6.21976077382285,-0.166732877511574,
-0.130251970586776));
#11201=CARTESIAN_POINT('Ctrl Pts',(6.2062585496807,-0.182517999394844,-0.107475484252795));
#11202=CARTESIAN_POINT('Ctrl Pts',(6.19025276528819,-0.198712082533353,
-0.0693141634661022));
#11203=CARTESIAN_POINT('Ctrl Pts',(6.18566388614715,-0.202908887997328,
-0.0559106681449083));
#11204=CARTESIAN_POINT('Ctrl Pts',(6.17929909433067,-0.208554382393535,
-0.0283388251429182));
#11205=CARTESIAN_POINT('Ctrl Pts',(6.17755280904565,-0.21,-0.0141630178371274));
#11206=CARTESIAN_POINT('Ctrl Pts',(6.17755280904565,-0.21,0.0141630178371274));
#11207=CARTESIAN_POINT('Ctrl Pts',(6.17929909433067,-0.208554382393535,
0.0283388251429182));
#11208=CARTESIAN_POINT('Ctrl Pts',(6.18566388614715,-0.202908887997328,
0.0559106681449083));
#11209=CARTESIAN_POINT('Ctrl Pts',(6.19025276528819,-0.198712082533353,
0.0693141634661022));
#11210=CARTESIAN_POINT('Ctrl Pts',(6.2062585496807,-0.182517999394844,0.107475484252794));
#11211=CARTESIAN_POINT('Ctrl Pts',(6.21976077382285,-0.166732877511574,
0.130251970586776));
#11212=CARTESIAN_POINT('Ctrl Pts',(6.24289105896451,-0.130678518444188,
0.166306329654162));
#11213=CARTESIAN_POINT('Ctrl Pts',(6.25439841412767,-0.107860332287473,
0.182341144032028));
#11214=CARTESIAN_POINT('Ctrl Pts',(6.27050625247645,-0.0563806217319961,
0.204214038345313));
#11215=CARTESIAN_POINT('Ctrl Pts',(6.275,-0.0276636393226109,0.21));
#11216=CARTESIAN_POINT('Ctrl Pts',(6.275,6.24500451351651E-17,0.21));
#11217=CARTESIAN_POINT('Ctrl Pts',(6.275,3.46944695195361E-17,0.21));
#11218=CARTESIAN_POINT('Ctrl Pts',(6.275,0.027663639322611,0.21));
#11219=CARTESIAN_POINT('Ctrl Pts',(6.27050625247645,0.0563806217319961,
0.204214038345313));
#11220=CARTESIAN_POINT('Ctrl Pts',(6.25439841412767,0.107860332287473,0.182341144032028));
#11221=CARTESIAN_POINT('Ctrl Pts',(6.24289105896451,0.130678518444188,0.166306329654162));
#11222=CARTESIAN_POINT('Ctrl Pts',(6.21976077382285,0.166732877511574,0.130251970586776));
#11223=CARTESIAN_POINT('Ctrl Pts',(6.2062585496807,0.182517999394844,0.107475484252794));
#11224=CARTESIAN_POINT('Ctrl Pts',(6.19025276528819,0.198712082533353,0.0693141634661021));
#11225=CARTESIAN_POINT('Ctrl Pts',(6.18566388614715,0.202908887997328,0.0559106681449083));
#11226=CARTESIAN_POINT('Ctrl Pts',(6.17929909433067,0.208554382393535,0.0283388251429182));
#11227=CARTESIAN_POINT('Ctrl Pts',(6.17755280904565,0.21,0.0141630178371273));
#11228=CARTESIAN_POINT('Ctrl Pts',(6.17755280904565,0.21,-2.77555756156289E-17));
#11229=CARTESIAN_POINT('Origin',(-0.1,0.,0.));
#11230=CARTESIAN_POINT('',(0.,-2.57175827820944E-17,0.21));
#11231=CARTESIAN_POINT('Origin',(0.,0.,0.));
#11232=CARTESIAN_POINT('',(-0.1,-2.57175827820944E-17,0.21));
#11233=CARTESIAN_POINT('Origin',(-0.1,0.82,-0.3));
#11234=CARTESIAN_POINT('',(0.,0.82,-0.3));
#11235=CARTESIAN_POINT('',(0.,1.,-0.3));
#11236=CARTESIAN_POINT('',(0.,0.41,-0.3));
#11237=CARTESIAN_POINT('',(40.,0.82,-0.3));
#11238=CARTESIAN_POINT('',(-0.1,0.82,-0.3));
#11239=CARTESIAN_POINT('',(40.,1.,-0.3));
#11240=CARTESIAN_POINT('',(40.,0.41,-0.3));
#11241=CARTESIAN_POINT('',(-0.05,1.,-0.3));
#11242=CARTESIAN_POINT('Origin',(-0.1,0.82,-0.55));
#11243=CARTESIAN_POINT('',(0.,0.82,-0.55));
#11244=CARTESIAN_POINT('',(0.,0.82,-0.275));
#11245=CARTESIAN_POINT('',(40.,0.82,-0.55));
#11246=CARTESIAN_POINT('',(-0.1,0.82,-0.55));
#11247=CARTESIAN_POINT('',(40.,0.82,-0.275));
#11248=CARTESIAN_POINT('Origin',(-0.1,0.67,-0.55));
#11249=CARTESIAN_POINT('',(0.,0.67,-0.55));
#11250=CARTESIAN_POINT('',(0.,0.335,-0.55));
#11251=CARTESIAN_POINT('',(40.,0.67,-0.55));
#11252=CARTESIAN_POINT('',(-0.1,0.67,-0.55));
#11253=CARTESIAN_POINT('',(40.,0.335,-0.55));
#11254=CARTESIAN_POINT('Origin',(-0.1,0.42,-0.3));
#11255=CARTESIAN_POINT('',(0.,0.42,-0.3));
#11256=CARTESIAN_POINT('',(0.,0.24,-0.12));
#11257=CARTESIAN_POINT('',(40.,0.42,-0.3));
#11258=CARTESIAN_POINT('',(-0.1,0.42,-0.3));
#11259=CARTESIAN_POINT('',(40.,0.24,-0.12));
#11260=CARTESIAN_POINT('Origin',(-0.1,0.42,0.3));
#11261=CARTESIAN_POINT('',(0.,0.42,0.3));
#11262=CARTESIAN_POINT('',(0.,0.42,0.15));
#11263=CARTESIAN_POINT('',(40.,0.42,0.3));
#11264=CARTESIAN_POINT('',(-0.1,0.42,0.3));
#11265=CARTESIAN_POINT('',(40.,0.42,0.15));
#11266=CARTESIAN_POINT('Origin',(-0.1,0.67,0.55));
#11267=CARTESIAN_POINT('',(0.,0.67,0.55));
#11268=CARTESIAN_POINT('',(6.93889390390723E-18,0.365,0.245));
#11269=CARTESIAN_POINT('',(40.,0.67,0.55));
#11270=CARTESIAN_POINT('',(-0.1,0.67,0.55));
#11271=CARTESIAN_POINT('',(40.,0.365,0.245));
#11272=CARTESIAN_POINT('Origin',(-0.1,0.82,0.55));
#11273=CARTESIAN_POINT('',(0.,0.82,0.55));
#11274=CARTESIAN_POINT('',(0.,0.41,0.55));
#11275=CARTESIAN_POINT('',(40.,0.82,0.55));
#11276=CARTESIAN_POINT('',(-0.1,0.82,0.55));
#11277=CARTESIAN_POINT('',(40.,0.41,0.55));
#11278=CARTESIAN_POINT('Origin',(-0.1,0.82,0.3));
#11279=CARTESIAN_POINT('',(0.,0.82,0.3));
#11280=CARTESIAN_POINT('',(0.,0.82,0.15));
#11281=CARTESIAN_POINT('',(40.,0.82,0.3));
#11282=CARTESIAN_POINT('',(-0.1,0.82,0.3));
#11283=CARTESIAN_POINT('',(40.,0.82,0.15));
#11284=CARTESIAN_POINT('Origin',(-0.1,1.05,0.3));
#11285=CARTESIAN_POINT('',(0.,1.,0.3));
#11286=CARTESIAN_POINT('',(0.,0.525,0.3));
#11287=CARTESIAN_POINT('',(40.,1.,0.3));
#11288=CARTESIAN_POINT('',(-0.05,1.,0.3));
#11289=CARTESIAN_POINT('',(40.,0.525,0.3));
#11290=CARTESIAN_POINT('Origin',(-0.1,-0.3,-0.82));
#11291=CARTESIAN_POINT('',(0.,-0.3,-0.82));
#11292=CARTESIAN_POINT('',(0.,-0.3,-1.));
#11293=CARTESIAN_POINT('',(0.,-0.3,-0.41));
#11294=CARTESIAN_POINT('',(40.,-0.3,-0.82));
#11295=CARTESIAN_POINT('',(-0.1,-0.3,-0.82));
#11296=CARTESIAN_POINT('',(40.,-0.3,-1.));
#11297=CARTESIAN_POINT('',(40.,-0.3,-0.41));
#11298=CARTESIAN_POINT('',(-0.05,-0.3,-1.));
#11299=CARTESIAN_POINT('Origin',(-0.1,-0.55,-0.82));
#11300=CARTESIAN_POINT('',(0.,-0.55,-0.82));
#11301=CARTESIAN_POINT('',(0.,-0.275,-0.82));
#11302=CARTESIAN_POINT('',(40.,-0.55,-0.82));
#11303=CARTESIAN_POINT('',(-0.1,-0.55,-0.82));
#11304=CARTESIAN_POINT('',(40.,-0.275,-0.82));
#11305=CARTESIAN_POINT('Origin',(-0.1,-0.55,-0.67));
#11306=CARTESIAN_POINT('',(0.,-0.55,-0.67));
#11307=CARTESIAN_POINT('',(0.,-0.55,-0.335));
#11308=CARTESIAN_POINT('',(40.,-0.55,-0.67));
#11309=CARTESIAN_POINT('',(-0.1,-0.55,-0.67));
#11310=CARTESIAN_POINT('',(40.,-0.55,-0.335));
#11311=CARTESIAN_POINT('Origin',(-0.1,-0.3,-0.42));
#11312=CARTESIAN_POINT('',(0.,-0.3,-0.42));
#11313=CARTESIAN_POINT('',(0.,-0.12,-0.24));
#11314=CARTESIAN_POINT('',(40.,-0.3,-0.42));
#11315=CARTESIAN_POINT('',(-0.1,-0.3,-0.42));
#11316=CARTESIAN_POINT('',(40.,-0.12,-0.24));
#11317=CARTESIAN_POINT('Origin',(-0.1,0.3,-0.42));
#11318=CARTESIAN_POINT('',(0.,0.3,-0.42));
#11319=CARTESIAN_POINT('',(0.,0.15,-0.42));
#11320=CARTESIAN_POINT('',(40.,0.3,-0.42));
#11321=CARTESIAN_POINT('',(-0.1,0.3,-0.42));
#11322=CARTESIAN_POINT('',(40.,0.15,-0.42));
#11323=CARTESIAN_POINT('Origin',(-0.1,0.55,-0.67));
#11324=CARTESIAN_POINT('',(0.,0.55,-0.67));
#11325=CARTESIAN_POINT('',(0.,0.245,-0.365));
#11326=CARTESIAN_POINT('',(40.,0.55,-0.67));
#11327=CARTESIAN_POINT('',(-0.1,0.55,-0.67));
#11328=CARTESIAN_POINT('',(40.,0.245,-0.365));
#11329=CARTESIAN_POINT('Origin',(-0.1,0.55,-0.82));
#11330=CARTESIAN_POINT('',(0.,0.55,-0.82));
#11331=CARTESIAN_POINT('',(0.,0.55,-0.41));
#11332=CARTESIAN_POINT('',(40.,0.55,-0.82));
#11333=CARTESIAN_POINT('',(-0.1,0.55,-0.82));
#11334=CARTESIAN_POINT('',(40.,0.55,-0.41));
#11335=CARTESIAN_POINT('Origin',(-0.1,0.3,-0.82));
#11336=CARTESIAN_POINT('',(0.,0.3,-0.82));
#11337=CARTESIAN_POINT('',(0.,0.15,-0.82));
#11338=CARTESIAN_POINT('',(40.,0.3,-0.82));
#11339=CARTESIAN_POINT('',(-0.1,0.3,-0.82));
#11340=CARTESIAN_POINT('',(40.,0.15,-0.82));
#11341=CARTESIAN_POINT('Origin',(-0.1,0.3,-1.05));
#11342=CARTESIAN_POINT('',(0.,0.3,-1.));
#11343=CARTESIAN_POINT('',(0.,0.3,-0.525));
#11344=CARTESIAN_POINT('',(40.,0.3,-1.));
#11345=CARTESIAN_POINT('',(-0.05,0.3,-1.));
#11346=CARTESIAN_POINT('',(40.,0.3,-0.525));
#11347=CARTESIAN_POINT('Origin',(-0.1,-0.82,0.3));
#11348=CARTESIAN_POINT('',(0.,-0.82,0.3));
#11349=CARTESIAN_POINT('',(0.,-1.,0.3));
#11350=CARTESIAN_POINT('',(0.,-0.41,0.3));
#11351=CARTESIAN_POINT('',(40.,-0.82,0.3));
#11352=CARTESIAN_POINT('',(-0.1,-0.82,0.3));
#11353=CARTESIAN_POINT('',(40.,-1.,0.3));
#11354=CARTESIAN_POINT('',(40.,-0.41,0.3));
#11355=CARTESIAN_POINT('',(-0.05,-1.,0.3));
#11356=CARTESIAN_POINT('Origin',(-0.1,-0.82,0.55));
#11357=CARTESIAN_POINT('',(0.,-0.82,0.55));
#11358=CARTESIAN_POINT('',(0.,-0.82,0.275));
#11359=CARTESIAN_POINT('',(40.,-0.82,0.55));
#11360=CARTESIAN_POINT('',(-0.1,-0.82,0.55));
#11361=CARTESIAN_POINT('',(40.,-0.82,0.275));
#11362=CARTESIAN_POINT('Origin',(-0.1,-0.67,0.55));
#11363=CARTESIAN_POINT('',(0.,-0.67,0.55));
#11364=CARTESIAN_POINT('',(0.,-0.335,0.55));
#11365=CARTESIAN_POINT('',(40.,-0.67,0.55));
#11366=CARTESIAN_POINT('',(-0.1,-0.67,0.55));
#11367=CARTESIAN_POINT('',(40.,-0.335,0.55));
#11368=CARTESIAN_POINT('Origin',(-0.1,-0.42,0.3));
#11369=CARTESIAN_POINT('',(0.,-0.42,0.3));
#11370=CARTESIAN_POINT('',(-6.93889390390723E-18,-0.24,0.12));
#11371=CARTESIAN_POINT('',(40.,-0.42,0.3));
#11372=CARTESIAN_POINT('',(-0.1,-0.42,0.3));
#11373=CARTESIAN_POINT('',(40.,-0.24,0.12));
#11374=CARTESIAN_POINT('Origin',(-0.1,-0.42,-0.3));
#11375=CARTESIAN_POINT('',(0.,-0.42,-0.3));
#11376=CARTESIAN_POINT('',(0.,-0.42,-0.15));
#11377=CARTESIAN_POINT('',(40.,-0.42,-0.3));
#11378=CARTESIAN_POINT('',(-0.1,-0.42,-0.3));
#11379=CARTESIAN_POINT('',(40.,-0.42,-0.15));
#11380=CARTESIAN_POINT('Origin',(-0.1,-0.67,-0.55));
#11381=CARTESIAN_POINT('',(0.,-0.67,-0.55));
#11382=CARTESIAN_POINT('',(0.,-0.365,-0.245));
#11383=CARTESIAN_POINT('',(40.,-0.67,-0.55));
#11384=CARTESIAN_POINT('',(-0.1,-0.67,-0.55));
#11385=CARTESIAN_POINT('',(40.,-0.365,-0.245));
#11386=CARTESIAN_POINT('Origin',(-0.1,-0.82,-0.55));
#11387=CARTESIAN_POINT('',(0.,-0.82,-0.55));
#11388=CARTESIAN_POINT('',(0.,-0.41,-0.55));
#11389=CARTESIAN_POINT('',(40.,-0.82,-0.55));
#11390=CARTESIAN_POINT('',(-0.1,-0.82,-0.55));
#11391=CARTESIAN_POINT('',(40.,-0.41,-0.55));
#11392=CARTESIAN_POINT('Origin',(-0.1,-0.82,-0.3));
#11393=CARTESIAN_POINT('',(0.,-0.82,-0.3));
#11394=CARTESIAN_POINT('',(0.,-0.82,-0.15));
#11395=CARTESIAN_POINT('',(40.,-0.82,-0.3));
#11396=CARTESIAN_POINT('',(-0.1,-0.82,-0.3));
#11397=CARTESIAN_POINT('',(40.,-0.82,-0.15));
#11398=CARTESIAN_POINT('Origin',(-0.1,-1.05,-0.3));
#11399=CARTESIAN_POINT('',(0.,-1.,-0.3));
#11400=CARTESIAN_POINT('',(0.,-0.525,-0.3));
#11401=CARTESIAN_POINT('',(40.,-1.,-0.3));
#11402=CARTESIAN_POINT('',(-0.05,-1.,-0.3));
#11403=CARTESIAN_POINT('',(40.,-0.525,-0.3));
#11404=CARTESIAN_POINT('Origin',(-0.1,0.3,0.82));
#11405=CARTESIAN_POINT('',(0.,0.3,0.82));
#11406=CARTESIAN_POINT('',(0.,0.3,1.));
#11407=CARTESIAN_POINT('',(0.,0.3,0.41));
#11408=CARTESIAN_POINT('',(40.,0.3,0.82));
#11409=CARTESIAN_POINT('',(-0.1,0.3,0.82));
#11410=CARTESIAN_POINT('',(40.,0.3,1.));
#11411=CARTESIAN_POINT('',(40.,0.3,0.41));
#11412=CARTESIAN_POINT('',(-0.05,0.3,1.));
#11413=CARTESIAN_POINT('Origin',(-0.1,0.55,0.82));
#11414=CARTESIAN_POINT('',(0.,0.55,0.82));
#11415=CARTESIAN_POINT('',(0.,0.275,0.82));
#11416=CARTESIAN_POINT('',(40.,0.55,0.82));
#11417=CARTESIAN_POINT('',(-0.1,0.55,0.82));
#11418=CARTESIAN_POINT('',(40.,0.275,0.82));
#11419=CARTESIAN_POINT('Origin',(-0.1,0.55,0.67));
#11420=CARTESIAN_POINT('',(0.,0.55,0.67));
#11421=CARTESIAN_POINT('',(0.,0.55,0.335));
#11422=CARTESIAN_POINT('',(40.,0.55,0.67));
#11423=CARTESIAN_POINT('',(-0.1,0.55,0.67));
#11424=CARTESIAN_POINT('',(40.,0.55,0.335));
#11425=CARTESIAN_POINT('Origin',(-0.1,0.3,0.42));
#11426=CARTESIAN_POINT('',(0.,0.3,0.42));
#11427=CARTESIAN_POINT('',(6.93889390390723E-18,0.12,0.24));
#11428=CARTESIAN_POINT('',(40.,0.3,0.42));
#11429=CARTESIAN_POINT('',(-0.1,0.3,0.42));
#11430=CARTESIAN_POINT('',(40.,0.12,0.24));
#11431=CARTESIAN_POINT('Origin',(-0.1,-0.3,0.42));
#11432=CARTESIAN_POINT('',(0.,-0.3,0.42));
#11433=CARTESIAN_POINT('',(0.,-0.15,0.42));
#11434=CARTESIAN_POINT('',(40.,-0.3,0.42));
#11435=CARTESIAN_POINT('',(-0.1,-0.3,0.42));
#11436=CARTESIAN_POINT('',(40.,-0.15,0.42));
#11437=CARTESIAN_POINT('Origin',(-0.1,-0.55,0.67));
#11438=CARTESIAN_POINT('',(0.,-0.55,0.67));
#11439=CARTESIAN_POINT('',(6.93889390390723E-18,-0.245,0.365));
#11440=CARTESIAN_POINT('',(40.,-0.55,0.67));
#11441=CARTESIAN_POINT('',(-0.1,-0.55,0.67));
#11442=CARTESIAN_POINT('',(40.,-0.245,0.365));
#11443=CARTESIAN_POINT('Origin',(-0.1,-0.55,0.82));
#11444=CARTESIAN_POINT('',(0.,-0.55,0.82));
#11445=CARTESIAN_POINT('',(0.,-0.55,0.41));
#11446=CARTESIAN_POINT('',(40.,-0.55,0.82));
#11447=CARTESIAN_POINT('',(-0.1,-0.55,0.82));
#11448=CARTESIAN_POINT('',(40.,-0.55,0.41));
#11449=CARTESIAN_POINT('Origin',(-0.1,-0.3,0.82));
#11450=CARTESIAN_POINT('',(0.,-0.3,0.82));
#11451=CARTESIAN_POINT('',(0.,-0.15,0.82));
#11452=CARTESIAN_POINT('',(40.,-0.3,0.82));
#11453=CARTESIAN_POINT('',(-0.1,-0.3,0.82));
#11454=CARTESIAN_POINT('',(40.,-0.15,0.82));
#11455=CARTESIAN_POINT('Origin',(-0.1,-0.3,1.05));
#11456=CARTESIAN_POINT('',(0.,-0.3,1.));
#11457=CARTESIAN_POINT('',(0.,-0.3,0.525));
#11458=CARTESIAN_POINT('',(40.,-0.3,1.));
#11459=CARTESIAN_POINT('',(-0.05,-0.3,1.));
#11460=CARTESIAN_POINT('',(40.,-0.3,0.525));
#11461=CARTESIAN_POINT('Origin',(-0.1,0.,0.));
#11462=CARTESIAN_POINT('',(40.,2.57175827820944E-17,0.21));
#11463=CARTESIAN_POINT('',(-0.1,-2.57175827820944E-17,0.21));
#11464=CARTESIAN_POINT('Origin',(40.,0.,0.));
#11465=CARTESIAN_POINT('Origin',(0.,1.,-1.));
#11466=CARTESIAN_POINT('',(0.,1.,1.));
#11467=CARTESIAN_POINT('',(0.,1.,-1.));
#11468=CARTESIAN_POINT('',(40.,1.,1.));
#11469=CARTESIAN_POINT('',(0.,1.,1.));
#11470=CARTESIAN_POINT('',(40.,1.,-1.));
#11471=CARTESIAN_POINT('Origin',(0.,1.,-1.));
#11472=CARTESIAN_POINT('',(40.,1.,-1.));
#11473=CARTESIAN_POINT('',(40.,1.,-1.));
#11474=CARTESIAN_POINT('',(0.,1.,-1.));
#11475=CARTESIAN_POINT('',(0.,1.,-1.));
#11476=CARTESIAN_POINT('',(0.,1.,-1.));
#11477=CARTESIAN_POINT('Origin',(0.,-1.,-1.));
#11478=CARTESIAN_POINT('',(0.,-1.,-1.));
#11479=CARTESIAN_POINT('',(40.,-1.,-1.));
#11480=CARTESIAN_POINT('Origin',(0.,-1.,-1.));
#11481=CARTESIAN_POINT('',(40.,-1.,-1.));
#11482=CARTESIAN_POINT('',(40.,-1.,-1.));
#11483=CARTESIAN_POINT('',(0.,-1.,-1.));
#11484=CARTESIAN_POINT('',(0.,-1.,-1.));
#11485=CARTESIAN_POINT('',(0.,-1.,-1.));
#11486=CARTESIAN_POINT('Origin',(0.,-1.,1.));
#11487=CARTESIAN_POINT('',(0.,-1.,1.));
#11488=CARTESIAN_POINT('',(40.,-1.,1.));
#11489=CARTESIAN_POINT('Origin',(0.,-1.,1.));
#11490=CARTESIAN_POINT('',(40.,-1.,1.));
#11491=CARTESIAN_POINT('',(40.,-1.,1.));
#11492=CARTESIAN_POINT('',(0.,-1.,1.));
#11493=CARTESIAN_POINT('',(0.,-1.,1.));
#11494=CARTESIAN_POINT('',(0.,-1.,1.));
#11495=CARTESIAN_POINT('Origin',(0.,1.,1.));
#11496=CARTESIAN_POINT('',(0.,1.,1.));
#11497=CARTESIAN_POINT('',(40.,1.,1.));
#11498=CARTESIAN_POINT('Origin',(0.,1.,1.));
#11499=CARTESIAN_POINT('',(40.,1.,1.));
#11500=CARTESIAN_POINT('',(0.,1.,1.));
#11501=CARTESIAN_POINT('Origin',(40.,0.,0.));
#11502=CARTESIAN_POINT('Origin',(0.,0.,0.));
#11503=CARTESIAN_POINT('',(0.,0.,0.));
#11504=CARTESIAN_POINT('Origin',(14.,0.,-1.1));
#11505=CARTESIAN_POINT('',(13.725,-3.36777869765523E-17,-0.42));
#11506=CARTESIAN_POINT('Origin',(14.,0.,-0.42));
#11507=CARTESIAN_POINT('',(13.725,-4.28597456279282E-17,-0.21));
#11508=CARTESIAN_POINT('',(13.725,-3.36777869765523E-17,-1.1));
#11509=CARTESIAN_POINT('',(13.725,-1.33694465363225E-17,0.21));
#11510=CARTESIAN_POINT('Ctrl Pts',(13.725,2.60208521396521E-17,0.21));
#11511=CARTESIAN_POINT('Ctrl Pts',(13.725,-0.027663639322611,0.21));
#11512=CARTESIAN_POINT('Ctrl Pts',(13.7294937475236,-0.0563806217319969,
0.204214038345313));
#11513=CARTESIAN_POINT('Ctrl Pts',(13.7456015858723,-0.107860332287474,
0.182341144032027));
#11514=CARTESIAN_POINT('Ctrl Pts',(13.7571089410355,-0.130678518444188,
0.166306329654162));
#11515=CARTESIAN_POINT('Ctrl Pts',(13.7802392261772,-0.166732877511574,
0.130251970586776));
#11516=CARTESIAN_POINT('Ctrl Pts',(13.7937414503193,-0.182517999394844,
0.107475484252795));
#11517=CARTESIAN_POINT('Ctrl Pts',(13.8097472347118,-0.198712082533353,
0.0693141634661024));
#11518=CARTESIAN_POINT('Ctrl Pts',(13.8143361138528,-0.202908887997328,
0.0559106681449082));
#11519=CARTESIAN_POINT('Ctrl Pts',(13.8207009056693,-0.208554382393535,
0.0283388251429175));
#11520=CARTESIAN_POINT('Ctrl Pts',(13.8224471909544,-0.21,0.0141630178371274));
#11521=CARTESIAN_POINT('Ctrl Pts',(13.8224471909544,-0.21,-0.0141630178371274));
#11522=CARTESIAN_POINT('Ctrl Pts',(13.8207009056693,-0.208554382393535,
-0.0283388251429175));
#11523=CARTESIAN_POINT('Ctrl Pts',(13.8143361138528,-0.202908887997328,
-0.0559106681449082));
#11524=CARTESIAN_POINT('Ctrl Pts',(13.8097472347118,-0.198712082533353,
-0.0693141634661024));
#11525=CARTESIAN_POINT('Ctrl Pts',(13.7937414503193,-0.182517999394844,
-0.107475484252795));
#11526=CARTESIAN_POINT('Ctrl Pts',(13.7802392261772,-0.166732877511574,
-0.130251970586776));
#11527=CARTESIAN_POINT('Ctrl Pts',(13.7571089410355,-0.130678518444188,
-0.166306329654162));
#11528=CARTESIAN_POINT('Ctrl Pts',(13.7456015858723,-0.107860332287474,
-0.182341144032027));
#11529=CARTESIAN_POINT('Ctrl Pts',(13.7294937475236,-0.0563806217319969,
-0.204214038345313));
#11530=CARTESIAN_POINT('Ctrl Pts',(13.725,-0.0276636393226111,-0.21));
#11531=CARTESIAN_POINT('Ctrl Pts',(13.725,-3.81639164714898E-17,-0.21));
#11532=CARTESIAN_POINT('',(13.725,3.36777869765523E-17,0.42));
#11533=CARTESIAN_POINT('',(13.725,-3.36777869765523E-17,-1.1));
#11534=CARTESIAN_POINT('Origin',(14.,0.,0.42));
#11535=CARTESIAN_POINT('',(13.8224471909544,0.21,6.93889390390723E-18));
#11536=CARTESIAN_POINT('Ctrl Pts',(13.8224471909544,0.21,6.93889390390723E-18));
#11537=CARTESIAN_POINT('Ctrl Pts',(13.8224471909544,0.21,0.0141630178371274));
#11538=CARTESIAN_POINT('Ctrl Pts',(13.8207009056693,0.208554382393535,0.0283388251429175));
#11539=CARTESIAN_POINT('Ctrl Pts',(13.8143361138528,0.202908887997328,0.0559106681449082));
#11540=CARTESIAN_POINT('Ctrl Pts',(13.8097472347118,0.198712082533353,0.0693141634661024));
#11541=CARTESIAN_POINT('Ctrl Pts',(13.7937414503193,0.182517999394844,0.107475484252795));
#11542=CARTESIAN_POINT('Ctrl Pts',(13.7802392261772,0.166732877511574,0.130251970586776));
#11543=CARTESIAN_POINT('Ctrl Pts',(13.7571089410355,0.130678518444188,0.166306329654162));
#11544=CARTESIAN_POINT('Ctrl Pts',(13.7456015858723,0.107860332287474,0.182341144032027));
#11545=CARTESIAN_POINT('Ctrl Pts',(13.7294937475236,0.056380621731997,0.204214038345313));
#11546=CARTESIAN_POINT('Ctrl Pts',(13.725,0.0276636393226111,0.21));
#11547=CARTESIAN_POINT('Ctrl Pts',(13.725,2.60208521396521E-17,0.21));
#11548=CARTESIAN_POINT('Ctrl Pts',(13.725,-8.32667268468867E-17,-0.21));
#11549=CARTESIAN_POINT('Ctrl Pts',(13.725,0.0276636393226109,-0.21));
#11550=CARTESIAN_POINT('Ctrl Pts',(13.7294937475236,0.0563806217319968,
-0.204214038345313));
#11551=CARTESIAN_POINT('Ctrl Pts',(13.7456015858723,0.107860332287474,-0.182341144032027));
#11552=CARTESIAN_POINT('Ctrl Pts',(13.7571089410355,0.130678518444188,-0.166306329654162));
#11553=CARTESIAN_POINT('Ctrl Pts',(13.7802392261772,0.166732877511574,-0.130251970586776));
#11554=CARTESIAN_POINT('Ctrl Pts',(13.7937414503193,0.182517999394844,-0.107475484252795));
#11555=CARTESIAN_POINT('Ctrl Pts',(13.8097472347118,0.198712082533353,-0.0693141634661024));
#11556=CARTESIAN_POINT('Ctrl Pts',(13.8143361138528,0.202908887997328,-0.0559106681449082));
#11557=CARTESIAN_POINT('Ctrl Pts',(13.8207009056693,0.208554382393535,-0.0283388251429175));
#11558=CARTESIAN_POINT('Ctrl Pts',(13.8224471909544,0.21,-0.0141630178371274));
#11559=CARTESIAN_POINT('Ctrl Pts',(13.8224471909544,0.21,-4.85722573273506E-17));
#11560=CARTESIAN_POINT('',(14.1775528090456,0.21,5.89805981832114E-17));
#11561=CARTESIAN_POINT('',(14.275,4.48844336872086E-18,0.21));
#11562=CARTESIAN_POINT('Ctrl Pts',(14.1775528090456,0.21,5.89805981832114E-17));
#11563=CARTESIAN_POINT('Ctrl Pts',(14.1775528090456,0.21,-0.0141630178371273));
#11564=CARTESIAN_POINT('Ctrl Pts',(14.1792990943307,0.208554382393535,-0.0283388251429175));
#11565=CARTESIAN_POINT('Ctrl Pts',(14.1856638861472,0.202908887997328,-0.0559106681449082));
#11566=CARTESIAN_POINT('Ctrl Pts',(14.1902527652882,0.198712082533353,-0.0693141634661024));
#11567=CARTESIAN_POINT('Ctrl Pts',(14.2062585496807,0.182517999394844,-0.107475484252795));
#11568=CARTESIAN_POINT('Ctrl Pts',(14.2197607738228,0.166732877511574,-0.130251970586776));
#11569=CARTESIAN_POINT('Ctrl Pts',(14.2428910589645,0.130678518444188,-0.166306329654162));
#11570=CARTESIAN_POINT('Ctrl Pts',(14.2543984141277,0.107860332287473,-0.182341144032028));
#11571=CARTESIAN_POINT('Ctrl Pts',(14.2705062524764,0.056380621731996,-0.204214038345313));
#11572=CARTESIAN_POINT('Ctrl Pts',(14.275,0.027663639322611,-0.21));
#11573=CARTESIAN_POINT('Ctrl Pts',(14.275,-0.0276636393226111,-0.21));
#11574=CARTESIAN_POINT('Ctrl Pts',(14.2705062524764,-0.0563806217319969,
-0.204214038345313));
#11575=CARTESIAN_POINT('Ctrl Pts',(14.2543984141277,-0.107860332287474,
-0.182341144032027));
#11576=CARTESIAN_POINT('Ctrl Pts',(14.2428910589645,-0.130678518444188,
-0.166306329654162));
#11577=CARTESIAN_POINT('Ctrl Pts',(14.2197607738228,-0.166732877511574,
-0.130251970586776));
#11578=CARTESIAN_POINT('Ctrl Pts',(14.2062585496807,-0.182517999394844,
-0.107475484252795));
#11579=CARTESIAN_POINT('Ctrl Pts',(14.1902527652882,-0.198712082533353,
-0.0693141634661024));
#11580=CARTESIAN_POINT('Ctrl Pts',(14.1856638861472,-0.202908887997328,
-0.0559106681449082));
#11581=CARTESIAN_POINT('Ctrl Pts',(14.1792990943307,-0.208554382393535,
-0.0283388251429175));
#11582=CARTESIAN_POINT('Ctrl Pts',(14.1775528090456,-0.21,-0.0141630178371274));
#11583=CARTESIAN_POINT('Ctrl Pts',(14.1775528090456,-0.21,0.0141630178371274));
#11584=CARTESIAN_POINT('Ctrl Pts',(14.1792990943307,-0.208554382393535,
0.0283388251429175));
#11585=CARTESIAN_POINT('Ctrl Pts',(14.1856638861472,-0.202908887997328,
0.0559106681449082));
#11586=CARTESIAN_POINT('Ctrl Pts',(14.1902527652882,-0.198712082533353,
0.0693141634661024));
#11587=CARTESIAN_POINT('Ctrl Pts',(14.2062585496807,-0.182517999394844,
0.107475484252795));
#11588=CARTESIAN_POINT('Ctrl Pts',(14.2197607738228,-0.166732877511574,
0.130251970586776));
#11589=CARTESIAN_POINT('Ctrl Pts',(14.2428910589645,-0.130678518444188,
0.166306329654162));
#11590=CARTESIAN_POINT('Ctrl Pts',(14.2543984141277,-0.107860332287474,
0.182341144032027));
#11591=CARTESIAN_POINT('Ctrl Pts',(14.2705062524764,-0.056380621731997,
0.204214038345313));
#11592=CARTESIAN_POINT('Ctrl Pts',(14.275,-0.0276636393226111,0.21));
#11593=CARTESIAN_POINT('Ctrl Pts',(14.275,-3.81639164714898E-17,0.21));
#11594=CARTESIAN_POINT('Ctrl Pts',(14.275,1.38777878078145E-17,0.21));
#11595=CARTESIAN_POINT('Ctrl Pts',(14.275,0.027663639322611,0.21));
#11596=CARTESIAN_POINT('Ctrl Pts',(14.2705062524764,0.0563806217319969,
0.204214038345313));
#11597=CARTESIAN_POINT('Ctrl Pts',(14.2543984141277,0.107860332287474,0.182341144032027));
#11598=CARTESIAN_POINT('Ctrl Pts',(14.2428910589645,0.130678518444188,0.166306329654162));
#11599=CARTESIAN_POINT('Ctrl Pts',(14.2197607738228,0.166732877511574,0.130251970586776));
#11600=CARTESIAN_POINT('Ctrl Pts',(14.2062585496807,0.182517999394844,0.107475484252795));
#11601=CARTESIAN_POINT('Ctrl Pts',(14.1902527652882,0.198712082533353,0.0693141634661024));
#11602=CARTESIAN_POINT('Ctrl Pts',(14.1856638861472,0.202908887997328,0.0559106681449082));
#11603=CARTESIAN_POINT('Ctrl Pts',(14.1792990943307,0.208554382393535,0.0283388251429175));
#11604=CARTESIAN_POINT('Ctrl Pts',(14.1775528090456,0.21,0.0141630178371274));
#11605=CARTESIAN_POINT('Ctrl Pts',(14.1775528090456,0.21,-1.38777878078145E-17));
#11606=CARTESIAN_POINT('Origin',(-0.1,0.,0.));
#11607=CARTESIAN_POINT('',(0.,-2.57175827820944E-17,0.21));
#11608=CARTESIAN_POINT('Origin',(0.,0.,0.));
#11609=CARTESIAN_POINT('',(-0.1,-2.57175827820944E-17,0.21));
#11610=CARTESIAN_POINT('Origin',(-0.1,0.82,-0.3));
#11611=CARTESIAN_POINT('',(0.,0.82,-0.3));
#11612=CARTESIAN_POINT('',(0.,1.,-0.3));
#11613=CARTESIAN_POINT('',(0.,0.41,-0.3));
#11614=CARTESIAN_POINT('',(20.,0.82,-0.3));
#11615=CARTESIAN_POINT('',(-0.1,0.82,-0.3));
#11616=CARTESIAN_POINT('',(20.,1.,-0.3));
#11617=CARTESIAN_POINT('',(20.,0.41,-0.3));
#11618=CARTESIAN_POINT('',(-0.05,1.,-0.3));
#11619=CARTESIAN_POINT('Origin',(-0.1,0.82,-0.55));
#11620=CARTESIAN_POINT('',(0.,0.82,-0.55));
#11621=CARTESIAN_POINT('',(0.,0.82,-0.275));
#11622=CARTESIAN_POINT('',(20.,0.82,-0.55));
#11623=CARTESIAN_POINT('',(-0.1,0.82,-0.55));
#11624=CARTESIAN_POINT('',(20.,0.82,-0.275));
#11625=CARTESIAN_POINT('Origin',(-0.1,0.67,-0.55));
#11626=CARTESIAN_POINT('',(0.,0.67,-0.55));
#11627=CARTESIAN_POINT('',(0.,0.335,-0.55));
#11628=CARTESIAN_POINT('',(20.,0.67,-0.55));
#11629=CARTESIAN_POINT('',(-0.1,0.67,-0.55));
#11630=CARTESIAN_POINT('',(20.,0.335,-0.55));
#11631=CARTESIAN_POINT('Origin',(-0.1,0.42,-0.3));
#11632=CARTESIAN_POINT('',(0.,0.42,-0.3));
#11633=CARTESIAN_POINT('',(0.,0.24,-0.12));
#11634=CARTESIAN_POINT('',(20.,0.42,-0.3));
#11635=CARTESIAN_POINT('',(-0.1,0.42,-0.3));
#11636=CARTESIAN_POINT('',(20.,0.24,-0.12));
#11637=CARTESIAN_POINT('Origin',(-0.1,0.42,0.3));
#11638=CARTESIAN_POINT('',(0.,0.42,0.3));
#11639=CARTESIAN_POINT('',(0.,0.42,0.15));
#11640=CARTESIAN_POINT('',(20.,0.42,0.3));
#11641=CARTESIAN_POINT('',(-0.1,0.42,0.3));
#11642=CARTESIAN_POINT('',(20.,0.42,0.15));
#11643=CARTESIAN_POINT('Origin',(-0.1,0.67,0.55));
#11644=CARTESIAN_POINT('',(0.,0.67,0.55));
#11645=CARTESIAN_POINT('',(6.93889390390723E-18,0.365,0.245));
#11646=CARTESIAN_POINT('',(20.,0.67,0.55));
#11647=CARTESIAN_POINT('',(-0.1,0.67,0.55));
#11648=CARTESIAN_POINT('',(20.,0.365,0.245));
#11649=CARTESIAN_POINT('Origin',(-0.1,0.82,0.55));
#11650=CARTESIAN_POINT('',(0.,0.82,0.55));
#11651=CARTESIAN_POINT('',(0.,0.41,0.55));
#11652=CARTESIAN_POINT('',(20.,0.82,0.55));
#11653=CARTESIAN_POINT('',(-0.1,0.82,0.55));
#11654=CARTESIAN_POINT('',(20.,0.41,0.55));
#11655=CARTESIAN_POINT('Origin',(-0.1,0.82,0.3));
#11656=CARTESIAN_POINT('',(0.,0.82,0.3));
#11657=CARTESIAN_POINT('',(0.,0.82,0.15));
#11658=CARTESIAN_POINT('',(20.,0.82,0.3));
#11659=CARTESIAN_POINT('',(-0.1,0.82,0.3));
#11660=CARTESIAN_POINT('',(20.,0.82,0.15));
#11661=CARTESIAN_POINT('Origin',(-0.1,1.05,0.3));
#11662=CARTESIAN_POINT('',(0.,1.,0.3));
#11663=CARTESIAN_POINT('',(0.,0.525,0.3));
#11664=CARTESIAN_POINT('',(20.,1.,0.3));
#11665=CARTESIAN_POINT('',(-0.05,1.,0.3));
#11666=CARTESIAN_POINT('',(20.,0.525,0.3));
#11667=CARTESIAN_POINT('Origin',(-0.1,-0.3,-0.82));
#11668=CARTESIAN_POINT('',(0.,-0.3,-0.82));
#11669=CARTESIAN_POINT('',(0.,-0.3,-1.));
#11670=CARTESIAN_POINT('',(0.,-0.3,-0.41));
#11671=CARTESIAN_POINT('',(20.,-0.3,-0.82));
#11672=CARTESIAN_POINT('',(-0.1,-0.3,-0.82));
#11673=CARTESIAN_POINT('',(20.,-0.3,-1.));
#11674=CARTESIAN_POINT('',(20.,-0.3,-0.41));
#11675=CARTESIAN_POINT('',(-0.05,-0.3,-1.));
#11676=CARTESIAN_POINT('Origin',(-0.1,-0.55,-0.82));
#11677=CARTESIAN_POINT('',(0.,-0.55,-0.82));
#11678=CARTESIAN_POINT('',(0.,-0.275,-0.82));
#11679=CARTESIAN_POINT('',(20.,-0.55,-0.82));
#11680=CARTESIAN_POINT('',(-0.1,-0.55,-0.82));
#11681=CARTESIAN_POINT('',(20.,-0.275,-0.82));
#11682=CARTESIAN_POINT('Origin',(-0.1,-0.55,-0.67));
#11683=CARTESIAN_POINT('',(0.,-0.55,-0.67));
#11684=CARTESIAN_POINT('',(0.,-0.55,-0.335));
#11685=CARTESIAN_POINT('',(20.,-0.55,-0.67));
#11686=CARTESIAN_POINT('',(-0.1,-0.55,-0.67));
#11687=CARTESIAN_POINT('',(20.,-0.55,-0.335));
#11688=CARTESIAN_POINT('Origin',(-0.1,-0.3,-0.42));
#11689=CARTESIAN_POINT('',(0.,-0.3,-0.42));
#11690=CARTESIAN_POINT('',(0.,-0.12,-0.24));
#11691=CARTESIAN_POINT('',(20.,-0.3,-0.42));
#11692=CARTESIAN_POINT('',(-0.1,-0.3,-0.42));
#11693=CARTESIAN_POINT('',(20.,-0.12,-0.24));
#11694=CARTESIAN_POINT('Origin',(-0.1,0.3,-0.42));
#11695=CARTESIAN_POINT('',(0.,0.3,-0.42));
#11696=CARTESIAN_POINT('',(0.,0.15,-0.42));
#11697=CARTESIAN_POINT('',(20.,0.3,-0.42));
#11698=CARTESIAN_POINT('',(-0.1,0.3,-0.42));
#11699=CARTESIAN_POINT('',(20.,0.15,-0.42));
#11700=CARTESIAN_POINT('Origin',(-0.1,0.55,-0.67));
#11701=CARTESIAN_POINT('',(0.,0.55,-0.67));
#11702=CARTESIAN_POINT('',(0.,0.245,-0.365));
#11703=CARTESIAN_POINT('',(20.,0.55,-0.67));
#11704=CARTESIAN_POINT('',(-0.1,0.55,-0.67));
#11705=CARTESIAN_POINT('',(20.,0.245,-0.365));
#11706=CARTESIAN_POINT('Origin',(-0.1,0.55,-0.82));
#11707=CARTESIAN_POINT('',(0.,0.55,-0.82));
#11708=CARTESIAN_POINT('',(0.,0.55,-0.41));
#11709=CARTESIAN_POINT('',(20.,0.55,-0.82));
#11710=CARTESIAN_POINT('',(-0.1,0.55,-0.82));
#11711=CARTESIAN_POINT('',(20.,0.55,-0.41));
#11712=CARTESIAN_POINT('Origin',(-0.1,0.3,-0.82));
#11713=CARTESIAN_POINT('',(0.,0.3,-0.82));
#11714=CARTESIAN_POINT('',(0.,0.15,-0.82));
#11715=CARTESIAN_POINT('',(20.,0.3,-0.82));
#11716=CARTESIAN_POINT('',(-0.1,0.3,-0.82));
#11717=CARTESIAN_POINT('',(20.,0.15,-0.82));
#11718=CARTESIAN_POINT('Origin',(-0.1,0.3,-1.05));
#11719=CARTESIAN_POINT('',(0.,0.3,-1.));
#11720=CARTESIAN_POINT('',(0.,0.3,-0.525));
#11721=CARTESIAN_POINT('',(20.,0.3,-1.));
#11722=CARTESIAN_POINT('',(-0.05,0.3,-1.));
#11723=CARTESIAN_POINT('',(20.,0.3,-0.525));
#11724=CARTESIAN_POINT('Origin',(-0.1,-0.82,0.3));
#11725=CARTESIAN_POINT('',(0.,-0.82,0.3));
#11726=CARTESIAN_POINT('',(0.,-1.,0.3));
#11727=CARTESIAN_POINT('',(0.,-0.41,0.3));
#11728=CARTESIAN_POINT('',(20.,-0.82,0.3));
#11729=CARTESIAN_POINT('',(-0.1,-0.82,0.3));
#11730=CARTESIAN_POINT('',(20.,-1.,0.3));
#11731=CARTESIAN_POINT('',(20.,-0.41,0.3));
#11732=CARTESIAN_POINT('',(-0.05,-1.,0.3));
#11733=CARTESIAN_POINT('Origin',(-0.1,-0.82,0.55));
#11734=CARTESIAN_POINT('',(0.,-0.82,0.55));
#11735=CARTESIAN_POINT('',(0.,-0.82,0.275));
#11736=CARTESIAN_POINT('',(20.,-0.82,0.55));
#11737=CARTESIAN_POINT('',(-0.1,-0.82,0.55));
#11738=CARTESIAN_POINT('',(20.,-0.82,0.275));
#11739=CARTESIAN_POINT('Origin',(-0.1,-0.67,0.55));
#11740=CARTESIAN_POINT('',(0.,-0.67,0.55));
#11741=CARTESIAN_POINT('',(0.,-0.335,0.55));
#11742=CARTESIAN_POINT('',(20.,-0.67,0.55));
#11743=CARTESIAN_POINT('',(-0.1,-0.67,0.55));
#11744=CARTESIAN_POINT('',(20.,-0.335,0.55));
#11745=CARTESIAN_POINT('Origin',(-0.1,-0.42,0.3));
#11746=CARTESIAN_POINT('',(0.,-0.42,0.3));
#11747=CARTESIAN_POINT('',(-6.93889390390723E-18,-0.24,0.12));
#11748=CARTESIAN_POINT('',(20.,-0.42,0.3));
#11749=CARTESIAN_POINT('',(-0.1,-0.42,0.3));
#11750=CARTESIAN_POINT('',(20.,-0.24,0.12));
#11751=CARTESIAN_POINT('Origin',(-0.1,-0.42,-0.3));
#11752=CARTESIAN_POINT('',(0.,-0.42,-0.3));
#11753=CARTESIAN_POINT('',(0.,-0.42,-0.15));
#11754=CARTESIAN_POINT('',(20.,-0.42,-0.3));
#11755=CARTESIAN_POINT('',(-0.1,-0.42,-0.3));
#11756=CARTESIAN_POINT('',(20.,-0.42,-0.15));
#11757=CARTESIAN_POINT('Origin',(-0.1,-0.67,-0.55));
#11758=CARTESIAN_POINT('',(0.,-0.67,-0.55));
#11759=CARTESIAN_POINT('',(0.,-0.365,-0.245));
#11760=CARTESIAN_POINT('',(20.,-0.67,-0.55));
#11761=CARTESIAN_POINT('',(-0.1,-0.67,-0.55));
#11762=CARTESIAN_POINT('',(20.,-0.365,-0.245));
#11763=CARTESIAN_POINT('Origin',(-0.1,-0.82,-0.55));
#11764=CARTESIAN_POINT('',(0.,-0.82,-0.55));
#11765=CARTESIAN_POINT('',(0.,-0.41,-0.55));
#11766=CARTESIAN_POINT('',(20.,-0.82,-0.55));
#11767=CARTESIAN_POINT('',(-0.1,-0.82,-0.55));
#11768=CARTESIAN_POINT('',(20.,-0.41,-0.55));
#11769=CARTESIAN_POINT('Origin',(-0.1,-0.82,-0.3));
#11770=CARTESIAN_POINT('',(0.,-0.82,-0.3));
#11771=CARTESIAN_POINT('',(0.,-0.82,-0.15));
#11772=CARTESIAN_POINT('',(20.,-0.82,-0.3));
#11773=CARTESIAN_POINT('',(-0.1,-0.82,-0.3));
#11774=CARTESIAN_POINT('',(20.,-0.82,-0.15));
#11775=CARTESIAN_POINT('Origin',(-0.1,-1.05,-0.3));
#11776=CARTESIAN_POINT('',(0.,-1.,-0.3));
#11777=CARTESIAN_POINT('',(0.,-0.525,-0.3));
#11778=CARTESIAN_POINT('',(20.,-1.,-0.3));
#11779=CARTESIAN_POINT('',(-0.05,-1.,-0.3));
#11780=CARTESIAN_POINT('',(20.,-0.525,-0.3));
#11781=CARTESIAN_POINT('Origin',(-0.1,0.3,0.82));
#11782=CARTESIAN_POINT('',(0.,0.3,0.82));
#11783=CARTESIAN_POINT('',(0.,0.3,1.));
#11784=CARTESIAN_POINT('',(0.,0.3,0.41));
#11785=CARTESIAN_POINT('',(20.,0.3,0.82));
#11786=CARTESIAN_POINT('',(-0.1,0.3,0.82));
#11787=CARTESIAN_POINT('',(20.,0.3,1.));
#11788=CARTESIAN_POINT('',(20.,0.3,0.41));
#11789=CARTESIAN_POINT('',(-0.05,0.3,1.));
#11790=CARTESIAN_POINT('Origin',(-0.1,0.55,0.82));
#11791=CARTESIAN_POINT('',(0.,0.55,0.82));
#11792=CARTESIAN_POINT('',(0.,0.275,0.82));
#11793=CARTESIAN_POINT('',(20.,0.55,0.82));
#11794=CARTESIAN_POINT('',(-0.1,0.55,0.82));
#11795=CARTESIAN_POINT('',(20.,0.275,0.82));
#11796=CARTESIAN_POINT('Origin',(-0.1,0.55,0.67));
#11797=CARTESIAN_POINT('',(0.,0.55,0.67));
#11798=CARTESIAN_POINT('',(0.,0.55,0.335));
#11799=CARTESIAN_POINT('',(20.,0.55,0.67));
#11800=CARTESIAN_POINT('',(-0.1,0.55,0.67));
#11801=CARTESIAN_POINT('',(20.,0.55,0.335));
#11802=CARTESIAN_POINT('Origin',(-0.1,0.3,0.42));
#11803=CARTESIAN_POINT('',(0.,0.3,0.42));
#11804=CARTESIAN_POINT('',(6.93889390390723E-18,0.12,0.24));
#11805=CARTESIAN_POINT('',(20.,0.3,0.42));
#11806=CARTESIAN_POINT('',(-0.1,0.3,0.42));
#11807=CARTESIAN_POINT('',(20.,0.12,0.24));
#11808=CARTESIAN_POINT('Origin',(-0.1,-0.3,0.42));
#11809=CARTESIAN_POINT('',(0.,-0.3,0.42));
#11810=CARTESIAN_POINT('',(0.,-0.15,0.42));
#11811=CARTESIAN_POINT('',(20.,-0.3,0.42));
#11812=CARTESIAN_POINT('',(-0.1,-0.3,0.42));
#11813=CARTESIAN_POINT('',(20.,-0.15,0.42));
#11814=CARTESIAN_POINT('Origin',(-0.1,-0.55,0.67));
#11815=CARTESIAN_POINT('',(0.,-0.55,0.67));
#11816=CARTESIAN_POINT('',(6.93889390390723E-18,-0.245,0.365));
#11817=CARTESIAN_POINT('',(20.,-0.55,0.67));
#11818=CARTESIAN_POINT('',(-0.1,-0.55,0.67));
#11819=CARTESIAN_POINT('',(20.,-0.245,0.365));
#11820=CARTESIAN_POINT('Origin',(-0.1,-0.55,0.82));
#11821=CARTESIAN_POINT('',(0.,-0.55,0.82));
#11822=CARTESIAN_POINT('',(0.,-0.55,0.41));
#11823=CARTESIAN_POINT('',(20.,-0.55,0.82));
#11824=CARTESIAN_POINT('',(-0.1,-0.55,0.82));
#11825=CARTESIAN_POINT('',(20.,-0.55,0.41));
#11826=CARTESIAN_POINT('Origin',(-0.1,-0.3,0.82));
#11827=CARTESIAN_POINT('',(0.,-0.3,0.82));
#11828=CARTESIAN_POINT('',(0.,-0.15,0.82));
#11829=CARTESIAN_POINT('',(20.,-0.3,0.82));
#11830=CARTESIAN_POINT('',(-0.1,-0.3,0.82));
#11831=CARTESIAN_POINT('',(20.,-0.15,0.82));
#11832=CARTESIAN_POINT('Origin',(-0.1,-0.3,1.05));
#11833=CARTESIAN_POINT('',(0.,-0.3,1.));
#11834=CARTESIAN_POINT('',(0.,-0.3,0.525));
#11835=CARTESIAN_POINT('',(20.,-0.3,1.));
#11836=CARTESIAN_POINT('',(-0.05,-0.3,1.));
#11837=CARTESIAN_POINT('',(20.,-0.3,0.525));
#11838=CARTESIAN_POINT('Origin',(-0.1,0.,0.));
#11839=CARTESIAN_POINT('',(20.,2.57175827820944E-17,0.21));
#11840=CARTESIAN_POINT('',(-0.1,-2.57175827820944E-17,0.21));
#11841=CARTESIAN_POINT('Origin',(20.,0.,0.));
#11842=CARTESIAN_POINT('Origin',(0.,1.,-1.));
#11843=CARTESIAN_POINT('',(0.,1.,1.));
#11844=CARTESIAN_POINT('',(0.,1.,-1.));
#11845=CARTESIAN_POINT('',(20.,1.,1.));
#11846=CARTESIAN_POINT('',(0.,1.,1.));
#11847=CARTESIAN_POINT('',(20.,1.,-1.));
#11848=CARTESIAN_POINT('Origin',(0.,1.,-1.));
#11849=CARTESIAN_POINT('',(20.,1.,-1.));
#11850=CARTESIAN_POINT('',(20.,1.,-1.));
#11851=CARTESIAN_POINT('',(0.,1.,-1.));
#11852=CARTESIAN_POINT('',(0.,1.,-1.));
#11853=CARTESIAN_POINT('',(0.,1.,-1.));
#11854=CARTESIAN_POINT('Origin',(0.,-1.,-1.));
#11855=CARTESIAN_POINT('',(0.,-1.,-1.));
#11856=CARTESIAN_POINT('',(20.,-1.,-1.));
#11857=CARTESIAN_POINT('Origin',(0.,-1.,-1.));
#11858=CARTESIAN_POINT('',(20.,-1.,-1.));
#11859=CARTESIAN_POINT('',(20.,-1.,-1.));
#11860=CARTESIAN_POINT('',(0.,-1.,-1.));
#11861=CARTESIAN_POINT('',(0.,-1.,-1.));
#11862=CARTESIAN_POINT('',(0.,-1.,-1.));
#11863=CARTESIAN_POINT('Origin',(0.,-1.,1.));
#11864=CARTESIAN_POINT('',(0.,-1.,1.));
#11865=CARTESIAN_POINT('',(20.,-1.,1.));
#11866=CARTESIAN_POINT('Origin',(0.,-1.,1.));
#11867=CARTESIAN_POINT('',(20.,-1.,1.));
#11868=CARTESIAN_POINT('',(20.,-1.,1.));
#11869=CARTESIAN_POINT('',(0.,-1.,1.));
#11870=CARTESIAN_POINT('',(0.,-1.,1.));
#11871=CARTESIAN_POINT('',(0.,-1.,1.));
#11872=CARTESIAN_POINT('Origin',(0.,1.,1.));
#11873=CARTESIAN_POINT('',(0.,1.,1.));
#11874=CARTESIAN_POINT('',(20.,1.,1.));
#11875=CARTESIAN_POINT('Origin',(0.,1.,1.));
#11876=CARTESIAN_POINT('',(20.,1.,1.));
#11877=CARTESIAN_POINT('',(0.,1.,1.));
#11878=CARTESIAN_POINT('Origin',(20.,0.,0.));
#11879=CARTESIAN_POINT('Origin',(0.,0.,0.));
#11880=CARTESIAN_POINT('',(0.,0.,0.));
#11881=CARTESIAN_POINT('Origin',(-0.1,0.82,-0.3));
#11882=CARTESIAN_POINT('',(0.,0.82,-0.3));
#11883=CARTESIAN_POINT('',(0.,1.,-0.3));
#11884=CARTESIAN_POINT('',(0.,0.41,-0.3));
#11885=CARTESIAN_POINT('',(20.,0.82,-0.3));
#11886=CARTESIAN_POINT('',(-0.1,0.82,-0.3));
#11887=CARTESIAN_POINT('',(20.,1.,-0.3));
#11888=CARTESIAN_POINT('',(20.,0.41,-0.3));
#11889=CARTESIAN_POINT('',(-0.05,1.,-0.3));
#11890=CARTESIAN_POINT('Origin',(-0.1,0.82,-0.55));
#11891=CARTESIAN_POINT('',(0.,0.82,-0.55));
#11892=CARTESIAN_POINT('',(0.,0.82,-0.275));
#11893=CARTESIAN_POINT('',(20.,0.82,-0.55));
#11894=CARTESIAN_POINT('',(-0.1,0.82,-0.55));
#11895=CARTESIAN_POINT('',(20.,0.82,-0.275));
#11896=CARTESIAN_POINT('Origin',(-0.1,0.67,-0.55));
#11897=CARTESIAN_POINT('',(0.,0.67,-0.55));
#11898=CARTESIAN_POINT('',(0.,0.335,-0.55));
#11899=CARTESIAN_POINT('',(20.,0.67,-0.55));
#11900=CARTESIAN_POINT('',(-0.1,0.67,-0.55));
#11901=CARTESIAN_POINT('',(20.,0.335,-0.55));
#11902=CARTESIAN_POINT('Origin',(-0.1,0.42,-0.3));
#11903=CARTESIAN_POINT('',(0.,0.42,-0.3));
#11904=CARTESIAN_POINT('',(0.,0.24,-0.12));
#11905=CARTESIAN_POINT('',(20.,0.42,-0.3));
#11906=CARTESIAN_POINT('',(-0.1,0.42,-0.3));
#11907=CARTESIAN_POINT('',(20.,0.24,-0.12));
#11908=CARTESIAN_POINT('Origin',(-0.1,0.42,0.3));
#11909=CARTESIAN_POINT('',(0.,0.42,0.3));
#11910=CARTESIAN_POINT('',(0.,0.42,0.15));
#11911=CARTESIAN_POINT('',(20.,0.42,0.3));
#11912=CARTESIAN_POINT('',(-0.1,0.42,0.3));
#11913=CARTESIAN_POINT('',(20.,0.42,0.15));
#11914=CARTESIAN_POINT('Origin',(-0.1,0.67,0.55));
#11915=CARTESIAN_POINT('',(0.,0.67,0.55));
#11916=CARTESIAN_POINT('',(6.93889390390723E-18,0.365,0.245));
#11917=CARTESIAN_POINT('',(20.,0.67,0.55));
#11918=CARTESIAN_POINT('',(-0.1,0.67,0.55));
#11919=CARTESIAN_POINT('',(20.,0.365,0.245));
#11920=CARTESIAN_POINT('Origin',(-0.1,0.82,0.55));
#11921=CARTESIAN_POINT('',(0.,0.82,0.55));
#11922=CARTESIAN_POINT('',(0.,0.41,0.55));
#11923=CARTESIAN_POINT('',(20.,0.82,0.55));
#11924=CARTESIAN_POINT('',(-0.1,0.82,0.55));
#11925=CARTESIAN_POINT('',(20.,0.41,0.55));
#11926=CARTESIAN_POINT('Origin',(-0.1,0.82,0.3));
#11927=CARTESIAN_POINT('',(0.,0.82,0.3));
#11928=CARTESIAN_POINT('',(0.,0.82,0.15));
#11929=CARTESIAN_POINT('',(20.,0.82,0.3));
#11930=CARTESIAN_POINT('',(-0.1,0.82,0.3));
#11931=CARTESIAN_POINT('',(20.,0.82,0.15));
#11932=CARTESIAN_POINT('Origin',(-0.1,1.05,0.3));
#11933=CARTESIAN_POINT('',(0.,1.,0.3));
#11934=CARTESIAN_POINT('',(0.,0.525,0.3));
#11935=CARTESIAN_POINT('',(20.,1.,0.3));
#11936=CARTESIAN_POINT('',(-0.05,1.,0.3));
#11937=CARTESIAN_POINT('',(20.,0.525,0.3));
#11938=CARTESIAN_POINT('Origin',(-0.1,-0.3,-0.82));
#11939=CARTESIAN_POINT('',(0.,-0.3,-0.82));
#11940=CARTESIAN_POINT('',(0.,-0.3,-1.));
#11941=CARTESIAN_POINT('',(0.,-0.3,-0.41));
#11942=CARTESIAN_POINT('',(20.,-0.3,-0.82));
#11943=CARTESIAN_POINT('',(-0.1,-0.3,-0.82));
#11944=CARTESIAN_POINT('',(20.,-0.3,-1.));
#11945=CARTESIAN_POINT('',(20.,-0.3,-0.41));
#11946=CARTESIAN_POINT('',(-0.05,-0.3,-1.));
#11947=CARTESIAN_POINT('Origin',(-0.1,-0.55,-0.82));
#11948=CARTESIAN_POINT('',(0.,-0.55,-0.82));
#11949=CARTESIAN_POINT('',(0.,-0.275,-0.82));
#11950=CARTESIAN_POINT('',(20.,-0.55,-0.82));
#11951=CARTESIAN_POINT('',(-0.1,-0.55,-0.82));
#11952=CARTESIAN_POINT('',(20.,-0.275,-0.82));
#11953=CARTESIAN_POINT('Origin',(-0.1,-0.55,-0.67));
#11954=CARTESIAN_POINT('',(0.,-0.55,-0.67));
#11955=CARTESIAN_POINT('',(0.,-0.55,-0.335));
#11956=CARTESIAN_POINT('',(20.,-0.55,-0.67));
#11957=CARTESIAN_POINT('',(-0.1,-0.55,-0.67));
#11958=CARTESIAN_POINT('',(20.,-0.55,-0.335));
#11959=CARTESIAN_POINT('Origin',(-0.1,-0.3,-0.42));
#11960=CARTESIAN_POINT('',(0.,-0.3,-0.42));
#11961=CARTESIAN_POINT('',(0.,-0.12,-0.24));
#11962=CARTESIAN_POINT('',(20.,-0.3,-0.42));
#11963=CARTESIAN_POINT('',(-0.1,-0.3,-0.42));
#11964=CARTESIAN_POINT('',(20.,-0.12,-0.24));
#11965=CARTESIAN_POINT('Origin',(-0.1,0.3,-0.42));
#11966=CARTESIAN_POINT('',(0.,0.3,-0.42));
#11967=CARTESIAN_POINT('',(0.,0.15,-0.42));
#11968=CARTESIAN_POINT('',(20.,0.3,-0.42));
#11969=CARTESIAN_POINT('',(-0.1,0.3,-0.42));
#11970=CARTESIAN_POINT('',(20.,0.15,-0.42));
#11971=CARTESIAN_POINT('Origin',(-0.1,0.55,-0.67));
#11972=CARTESIAN_POINT('',(0.,0.55,-0.67));
#11973=CARTESIAN_POINT('',(0.,0.245,-0.365));
#11974=CARTESIAN_POINT('',(20.,0.55,-0.67));
#11975=CARTESIAN_POINT('',(-0.1,0.55,-0.67));
#11976=CARTESIAN_POINT('',(20.,0.245,-0.365));
#11977=CARTESIAN_POINT('Origin',(-0.1,0.55,-0.82));
#11978=CARTESIAN_POINT('',(0.,0.55,-0.82));
#11979=CARTESIAN_POINT('',(0.,0.55,-0.41));
#11980=CARTESIAN_POINT('',(20.,0.55,-0.82));
#11981=CARTESIAN_POINT('',(-0.1,0.55,-0.82));
#11982=CARTESIAN_POINT('',(20.,0.55,-0.41));
#11983=CARTESIAN_POINT('Origin',(-0.1,0.3,-0.82));
#11984=CARTESIAN_POINT('',(0.,0.3,-0.82));
#11985=CARTESIAN_POINT('',(0.,0.15,-0.82));
#11986=CARTESIAN_POINT('',(20.,0.3,-0.82));
#11987=CARTESIAN_POINT('',(-0.1,0.3,-0.82));
#11988=CARTESIAN_POINT('',(20.,0.15,-0.82));
#11989=CARTESIAN_POINT('Origin',(-0.1,0.3,-1.05));
#11990=CARTESIAN_POINT('',(0.,0.3,-1.));
#11991=CARTESIAN_POINT('',(0.,0.3,-0.525));
#11992=CARTESIAN_POINT('',(20.,0.3,-1.));
#11993=CARTESIAN_POINT('',(-0.05,0.3,-1.));
#11994=CARTESIAN_POINT('',(20.,0.3,-0.525));
#11995=CARTESIAN_POINT('Origin',(-0.1,-0.82,0.3));
#11996=CARTESIAN_POINT('',(0.,-0.82,0.3));
#11997=CARTESIAN_POINT('',(0.,-1.,0.3));
#11998=CARTESIAN_POINT('',(0.,-0.41,0.3));
#11999=CARTESIAN_POINT('',(20.,-0.82,0.3));
#12000=CARTESIAN_POINT('',(-0.1,-0.82,0.3));
#12001=CARTESIAN_POINT('',(20.,-1.,0.3));
#12002=CARTESIAN_POINT('',(20.,-0.41,0.3));
#12003=CARTESIAN_POINT('',(-0.05,-1.,0.3));
#12004=CARTESIAN_POINT('Origin',(-0.1,-0.82,0.55));
#12005=CARTESIAN_POINT('',(0.,-0.82,0.55));
#12006=CARTESIAN_POINT('',(0.,-0.82,0.275));
#12007=CARTESIAN_POINT('',(20.,-0.82,0.55));
#12008=CARTESIAN_POINT('',(-0.1,-0.82,0.55));
#12009=CARTESIAN_POINT('',(20.,-0.82,0.275));
#12010=CARTESIAN_POINT('Origin',(-0.1,-0.67,0.55));
#12011=CARTESIAN_POINT('',(0.,-0.67,0.55));
#12012=CARTESIAN_POINT('',(0.,-0.335,0.55));
#12013=CARTESIAN_POINT('',(20.,-0.67,0.55));
#12014=CARTESIAN_POINT('',(-0.1,-0.67,0.55));
#12015=CARTESIAN_POINT('',(20.,-0.335,0.55));
#12016=CARTESIAN_POINT('Origin',(-0.1,-0.42,0.3));
#12017=CARTESIAN_POINT('',(0.,-0.42,0.3));
#12018=CARTESIAN_POINT('',(-6.93889390390723E-18,-0.24,0.12));
#12019=CARTESIAN_POINT('',(20.,-0.42,0.3));
#12020=CARTESIAN_POINT('',(-0.1,-0.42,0.3));
#12021=CARTESIAN_POINT('',(20.,-0.24,0.12));
#12022=CARTESIAN_POINT('Origin',(-0.1,-0.42,-0.3));
#12023=CARTESIAN_POINT('',(0.,-0.42,-0.3));
#12024=CARTESIAN_POINT('',(0.,-0.42,-0.15));
#12025=CARTESIAN_POINT('',(20.,-0.42,-0.3));
#12026=CARTESIAN_POINT('',(-0.1,-0.42,-0.3));
#12027=CARTESIAN_POINT('',(20.,-0.42,-0.15));
#12028=CARTESIAN_POINT('Origin',(-0.1,-0.67,-0.55));
#12029=CARTESIAN_POINT('',(0.,-0.67,-0.55));
#12030=CARTESIAN_POINT('',(0.,-0.365,-0.245));
#12031=CARTESIAN_POINT('',(20.,-0.67,-0.55));
#12032=CARTESIAN_POINT('',(-0.1,-0.67,-0.55));
#12033=CARTESIAN_POINT('',(20.,-0.365,-0.245));
#12034=CARTESIAN_POINT('Origin',(-0.1,-0.82,-0.55));
#12035=CARTESIAN_POINT('',(0.,-0.82,-0.55));
#12036=CARTESIAN_POINT('',(0.,-0.41,-0.55));
#12037=CARTESIAN_POINT('',(20.,-0.82,-0.55));
#12038=CARTESIAN_POINT('',(-0.1,-0.82,-0.55));
#12039=CARTESIAN_POINT('',(20.,-0.41,-0.55));
#12040=CARTESIAN_POINT('Origin',(-0.1,-0.82,-0.3));
#12041=CARTESIAN_POINT('',(0.,-0.82,-0.3));
#12042=CARTESIAN_POINT('',(0.,-0.82,-0.15));
#12043=CARTESIAN_POINT('',(20.,-0.82,-0.3));
#12044=CARTESIAN_POINT('',(-0.1,-0.82,-0.3));
#12045=CARTESIAN_POINT('',(20.,-0.82,-0.15));
#12046=CARTESIAN_POINT('Origin',(-0.1,-1.05,-0.3));
#12047=CARTESIAN_POINT('',(0.,-1.,-0.3));
#12048=CARTESIAN_POINT('',(0.,-0.525,-0.3));
#12049=CARTESIAN_POINT('',(20.,-1.,-0.3));
#12050=CARTESIAN_POINT('',(-0.05,-1.,-0.3));
#12051=CARTESIAN_POINT('',(20.,-0.525,-0.3));
#12052=CARTESIAN_POINT('Origin',(-0.1,0.3,0.82));
#12053=CARTESIAN_POINT('',(0.,0.3,0.82));
#12054=CARTESIAN_POINT('',(0.,0.3,1.));
#12055=CARTESIAN_POINT('',(0.,0.3,0.41));
#12056=CARTESIAN_POINT('',(20.,0.3,0.82));
#12057=CARTESIAN_POINT('',(-0.1,0.3,0.82));
#12058=CARTESIAN_POINT('',(20.,0.3,1.));
#12059=CARTESIAN_POINT('',(20.,0.3,0.41));
#12060=CARTESIAN_POINT('',(-0.05,0.3,1.));
#12061=CARTESIAN_POINT('Origin',(-0.1,0.55,0.82));
#12062=CARTESIAN_POINT('',(0.,0.55,0.82));
#12063=CARTESIAN_POINT('',(0.,0.275,0.82));
#12064=CARTESIAN_POINT('',(20.,0.55,0.82));
#12065=CARTESIAN_POINT('',(-0.1,0.55,0.82));
#12066=CARTESIAN_POINT('',(20.,0.275,0.82));
#12067=CARTESIAN_POINT('Origin',(-0.1,0.55,0.67));
#12068=CARTESIAN_POINT('',(0.,0.55,0.67));
#12069=CARTESIAN_POINT('',(0.,0.55,0.335));
#12070=CARTESIAN_POINT('',(20.,0.55,0.67));
#12071=CARTESIAN_POINT('',(-0.1,0.55,0.67));
#12072=CARTESIAN_POINT('',(20.,0.55,0.335));
#12073=CARTESIAN_POINT('Origin',(-0.1,0.3,0.42));
#12074=CARTESIAN_POINT('',(0.,0.3,0.42));
#12075=CARTESIAN_POINT('',(6.93889390390723E-18,0.12,0.24));
#12076=CARTESIAN_POINT('',(20.,0.3,0.42));
#12077=CARTESIAN_POINT('',(-0.1,0.3,0.42));
#12078=CARTESIAN_POINT('',(20.,0.12,0.24));
#12079=CARTESIAN_POINT('Origin',(-0.1,-0.3,0.42));
#12080=CARTESIAN_POINT('',(0.,-0.3,0.42));
#12081=CARTESIAN_POINT('',(0.,-0.15,0.42));
#12082=CARTESIAN_POINT('',(20.,-0.3,0.42));
#12083=CARTESIAN_POINT('',(-0.1,-0.3,0.42));
#12084=CARTESIAN_POINT('',(20.,-0.15,0.42));
#12085=CARTESIAN_POINT('Origin',(-0.1,-0.55,0.67));
#12086=CARTESIAN_POINT('',(0.,-0.55,0.67));
#12087=CARTESIAN_POINT('',(6.93889390390723E-18,-0.245,0.365));
#12088=CARTESIAN_POINT('',(20.,-0.55,0.67));
#12089=CARTESIAN_POINT('',(-0.1,-0.55,0.67));
#12090=CARTESIAN_POINT('',(20.,-0.245,0.365));
#12091=CARTESIAN_POINT('Origin',(-0.1,-0.55,0.82));
#12092=CARTESIAN_POINT('',(0.,-0.55,0.82));
#12093=CARTESIAN_POINT('',(0.,-0.55,0.41));
#12094=CARTESIAN_POINT('',(20.,-0.55,0.82));
#12095=CARTESIAN_POINT('',(-0.1,-0.55,0.82));
#12096=CARTESIAN_POINT('',(20.,-0.55,0.41));
#12097=CARTESIAN_POINT('Origin',(-0.1,-0.3,0.82));
#12098=CARTESIAN_POINT('',(0.,-0.3,0.82));
#12099=CARTESIAN_POINT('',(0.,-0.15,0.82));
#12100=CARTESIAN_POINT('',(20.,-0.3,0.82));
#12101=CARTESIAN_POINT('',(-0.1,-0.3,0.82));
#12102=CARTESIAN_POINT('',(20.,-0.15,0.82));
#12103=CARTESIAN_POINT('Origin',(-0.1,-0.3,1.05));
#12104=CARTESIAN_POINT('',(0.,-0.3,1.));
#12105=CARTESIAN_POINT('',(0.,-0.3,0.525));
#12106=CARTESIAN_POINT('',(20.,-0.3,1.));
#12107=CARTESIAN_POINT('',(-0.05,-0.3,1.));
#12108=CARTESIAN_POINT('',(20.,-0.3,0.525));
#12109=CARTESIAN_POINT('Origin',(-0.1,0.,0.));
#12110=CARTESIAN_POINT('',(0.,-2.57175827820944E-17,0.21));
#12111=CARTESIAN_POINT('Origin',(0.,0.,0.));
#12112=CARTESIAN_POINT('',(20.,2.57175827820944E-17,0.21));
#12113=CARTESIAN_POINT('',(-0.1,-2.57175827820944E-17,0.21));
#12114=CARTESIAN_POINT('Origin',(20.,0.,0.));
#12115=CARTESIAN_POINT('Origin',(0.,1.,-1.));
#12116=CARTESIAN_POINT('',(0.,1.,1.));
#12117=CARTESIAN_POINT('',(0.,1.,-1.));
#12118=CARTESIAN_POINT('',(20.,1.,1.));
#12119=CARTESIAN_POINT('',(0.,1.,1.));
#12120=CARTESIAN_POINT('',(20.,1.,-1.));
#12121=CARTESIAN_POINT('Origin',(0.,1.,-1.));
#12122=CARTESIAN_POINT('',(20.,1.,-1.));
#12123=CARTESIAN_POINT('',(20.,1.,-1.));
#12124=CARTESIAN_POINT('',(0.,1.,-1.));
#12125=CARTESIAN_POINT('',(0.,1.,-1.));
#12126=CARTESIAN_POINT('',(0.,1.,-1.));
#12127=CARTESIAN_POINT('Origin',(0.,-1.,-1.));
#12128=CARTESIAN_POINT('',(0.,-1.,-1.));
#12129=CARTESIAN_POINT('',(20.,-1.,-1.));
#12130=CARTESIAN_POINT('Origin',(0.,-1.,-1.));
#12131=CARTESIAN_POINT('',(20.,-1.,-1.));
#12132=CARTESIAN_POINT('',(20.,-1.,-1.));
#12133=CARTESIAN_POINT('',(0.,-1.,-1.));
#12134=CARTESIAN_POINT('',(0.,-1.,-1.));
#12135=CARTESIAN_POINT('',(0.,-1.,-1.));
#12136=CARTESIAN_POINT('Origin',(0.,-1.,1.));
#12137=CARTESIAN_POINT('',(0.,-1.,1.));
#12138=CARTESIAN_POINT('',(20.,-1.,1.));
#12139=CARTESIAN_POINT('Origin',(0.,-1.,1.));
#12140=CARTESIAN_POINT('',(20.,-1.,1.));
#12141=CARTESIAN_POINT('',(20.,-1.,1.));
#12142=CARTESIAN_POINT('',(0.,-1.,1.));
#12143=CARTESIAN_POINT('',(0.,-1.,1.));
#12144=CARTESIAN_POINT('',(0.,-1.,1.));
#12145=CARTESIAN_POINT('Origin',(0.,1.,1.));
#12146=CARTESIAN_POINT('',(0.,1.,1.));
#12147=CARTESIAN_POINT('',(20.,1.,1.));
#12148=CARTESIAN_POINT('Origin',(0.,1.,1.));
#12149=CARTESIAN_POINT('',(20.,1.,1.));
#12150=CARTESIAN_POINT('',(0.,1.,1.));
#12151=CARTESIAN_POINT('Origin',(20.,0.,0.));
#12152=CARTESIAN_POINT('Origin',(0.,0.,0.));
#12153=CARTESIAN_POINT('',(0.,0.,0.));
#12154=CARTESIAN_POINT('Origin',(0.115470053837925,-0.5,-0.2));
#12155=CARTESIAN_POINT('',(0.23094010767585,-0.5,0.));
#12156=CARTESIAN_POINT('',(0.115470053837925,-0.5,-0.2));
#12157=CARTESIAN_POINT('',(0.23094010767585,-0.5,0.));
#12158=CARTESIAN_POINT('',(0.115470053837925,-0.8,-0.2));
#12159=CARTESIAN_POINT('',(0.115470053837925,-0.5,-0.2));
#12160=CARTESIAN_POINT('',(0.23094010767585,-0.8,0.));
#12161=CARTESIAN_POINT('',(0.23094010767585,-0.8,0.));
#12162=CARTESIAN_POINT('',(0.23094010767585,-0.5,0.));
#12163=CARTESIAN_POINT('Origin',(-0.115470053837925,-0.5,-0.2));
#12164=CARTESIAN_POINT('',(-0.115470053837925,-0.5,-0.2));
#12165=CARTESIAN_POINT('',(0.115470053837925,-0.5,-0.2));
#12166=CARTESIAN_POINT('',(-0.115470053837925,-0.8,-0.2));
#12167=CARTESIAN_POINT('',(-0.115470053837925,-0.5,-0.2));
#12168=CARTESIAN_POINT('',(0.115470053837925,-0.8,-0.2));
#12169=CARTESIAN_POINT('Origin',(-0.23094010767585,-0.5,-2.77555756156289E-17));
#12170=CARTESIAN_POINT('',(-0.23094010767585,-0.5,-2.82820063659975E-17));
#12171=CARTESIAN_POINT('',(-0.115470053837925,-0.5,-0.2));
#12172=CARTESIAN_POINT('',(-0.23094010767585,-0.8,-2.77555756156289E-17));
#12173=CARTESIAN_POINT('',(-0.23094010767585,-0.5,-2.82820063659975E-17));
#12174=CARTESIAN_POINT('',(-0.115470053837925,-0.8,-0.2));
#12175=CARTESIAN_POINT('Origin',(-0.115470053837925,-0.5,0.2));
#12176=CARTESIAN_POINT('',(-0.115470053837925,-0.5,0.2));
#12177=CARTESIAN_POINT('',(-0.23094010767585,-0.5,-2.82820063659975E-17));
#12178=CARTESIAN_POINT('',(-0.115470053837925,-0.8,0.2));
#12179=CARTESIAN_POINT('',(-0.115470053837925,-0.5,0.2));
#12180=CARTESIAN_POINT('',(-0.23094010767585,-0.8,-2.82820063659975E-17));
#12181=CARTESIAN_POINT('Origin',(0.115470053837925,-0.5,0.2));
#12182=CARTESIAN_POINT('',(0.115470053837925,-0.5,0.2));
#12183=CARTESIAN_POINT('',(-0.115470053837925,-0.5,0.2));
#12184=CARTESIAN_POINT('',(0.115470053837925,-0.8,0.2));
#12185=CARTESIAN_POINT('',(0.115470053837925,-0.5,0.2));
#12186=CARTESIAN_POINT('',(-0.115470053837925,-0.8,0.2));
#12187=CARTESIAN_POINT('Origin',(0.23094010767585,-0.5,0.));
#12188=CARTESIAN_POINT('',(0.115470053837925,-0.5,0.2));
#12189=CARTESIAN_POINT('',(0.115470053837925,-0.8,0.2));
#12190=CARTESIAN_POINT('Origin',(0.,-0.5,0.));
#12191=CARTESIAN_POINT('Origin',(0.,-0.8,0.));
#12192=CARTESIAN_POINT('Origin',(0.,-1.9,0.));
#12193=CARTESIAN_POINT('',(-0.25,-1.9,3.06161699786838E-17));
#12194=CARTESIAN_POINT('Origin',(0.,-1.9,0.));
#12195=CARTESIAN_POINT('',(-0.24505,-1.9,3.00099698131059E-17));
#12196=CARTESIAN_POINT('Origin',(0.,-1.9,0.));
#12197=CARTESIAN_POINT('Origin',(0.,-4.,0.));
#12198=CARTESIAN_POINT('',(-0.25,-4.,3.06161699786838E-17));
#12199=CARTESIAN_POINT('',(-0.25,-4.,3.06161699786838E-17));
#12200=CARTESIAN_POINT('Origin',(0.,-4.,0.));
#12201=CARTESIAN_POINT('Origin',(0.,-4.,0.));
#12202=CARTESIAN_POINT('Origin',(0.375,0.5,0.));
#12203=CARTESIAN_POINT('',(-0.375,0.5,-4.59242549680257E-17));
#12204=CARTESIAN_POINT('Origin',(0.,0.5,0.));
#12205=CARTESIAN_POINT('Origin',(0.,0.475,0.));
#12206=CARTESIAN_POINT('',(-0.425,0.45,-5.20474889637625E-17));
#12207=CARTESIAN_POINT('Origin',(0.,0.45,0.));
#12208=CARTESIAN_POINT('',(-0.4,0.475,-4.89858719658941E-17));
#12209=CARTESIAN_POINT('Origin',(0.,0.24,0.));
#12210=CARTESIAN_POINT('',(-0.425,0.0299999999999998,-5.20474889637625E-17));
#12211=CARTESIAN_POINT('Origin',(0.,0.0299999999999998,0.));
#12212=CARTESIAN_POINT('',(-0.425,0.24,-5.20474889637625E-17));
#12213=CARTESIAN_POINT('Origin',(0.,0.0150000000000001,0.));
#12214=CARTESIAN_POINT('',(-0.395,4.85722573273506E-17,-4.83735485663204E-17));
#12215=CARTESIAN_POINT('Origin',(0.,0.,0.));
#12216=CARTESIAN_POINT('',(-0.41,0.0150000000000001,-5.02105187650415E-17));
#12217=CARTESIAN_POINT('Origin',(0.27,0.,0.));
#12218=CARTESIAN_POINT('',(-0.27,0.,-3.30654635769785E-17));
#12219=CARTESIAN_POINT('Origin',(0.,0.,0.));
#12220=CARTESIAN_POINT('Origin',(0.,-0.02,0.));
#12221=CARTESIAN_POINT('',(-0.24505,-0.0498999999999999,3.00099698131059E-17));
#12222=CARTESIAN_POINT('Origin',(0.,-0.0498999999999999,0.));
#12223=CARTESIAN_POINT('',(-0.26,-0.02,-3.18408167778312E-17));
#12224=CARTESIAN_POINT('Origin',(0.,-0.995,0.));
#12225=CARTESIAN_POINT('',(-0.24505,-0.995,-3.00099698131059E-17));
#12226=CARTESIAN_POINT('',(0.,0.,0.));
#12227=CARTESIAN_POINT('Origin',(0.375,0.5,0.));
#12228=CARTESIAN_POINT('',(-0.375,0.5,-4.59242549680257E-17));
#12229=CARTESIAN_POINT('Origin',(0.,0.5,0.));
#12230=CARTESIAN_POINT('Origin',(0.,0.475,0.));
#12231=CARTESIAN_POINT('',(-0.425,0.45,-5.20474889637625E-17));
#12232=CARTESIAN_POINT('Origin',(0.,0.45,0.));
#12233=CARTESIAN_POINT('',(-0.4,0.475,-4.89858719658941E-17));
#12234=CARTESIAN_POINT('Origin',(0.,0.24,0.));
#12235=CARTESIAN_POINT('',(-0.425,0.0299999999999998,-5.20474889637625E-17));
#12236=CARTESIAN_POINT('Origin',(0.,0.0299999999999998,0.));
#12237=CARTESIAN_POINT('',(-0.425,0.24,-5.20474889637625E-17));
#12238=CARTESIAN_POINT('Origin',(0.,0.0150000000000001,0.));
#12239=CARTESIAN_POINT('',(-0.395,4.85722573273506E-17,-4.83735485663204E-17));
#12240=CARTESIAN_POINT('Origin',(0.,0.,0.));
#12241=CARTESIAN_POINT('',(-0.41,0.0150000000000001,-5.02105187650415E-17));
#12242=CARTESIAN_POINT('Origin',(0.27,0.,0.));
#12243=CARTESIAN_POINT('',(-0.27,0.,-3.30654635769785E-17));
#12244=CARTESIAN_POINT('Origin',(0.,0.,0.));
#12245=CARTESIAN_POINT('Origin',(0.,-0.02,0.));
#12246=CARTESIAN_POINT('',(-0.24505,-0.0498999999999999,3.00099698131059E-17));
#12247=CARTESIAN_POINT('Origin',(0.,-0.0498999999999999,0.));
#12248=CARTESIAN_POINT('',(-0.26,-0.02,-3.18408167778312E-17));
#12249=CARTESIAN_POINT('Origin',(0.,-0.995,0.));
#12250=CARTESIAN_POINT('',(-0.24505,-1.95495,3.00099698131059E-17));
#12251=CARTESIAN_POINT('Origin',(0.,-1.95495,0.));
#12252=CARTESIAN_POINT('',(-0.24505,-0.995,-3.00099698131059E-17));
#12253=CARTESIAN_POINT('Origin',(0.,-1.975,0.));
#12254=CARTESIAN_POINT('',(-0.2,-2.,-2.44929359829471E-17));
#12255=CARTESIAN_POINT('Origin',(0.,-2.,0.));
#12256=CARTESIAN_POINT('',(-0.225,-1.975,-2.75545529808154E-17));
#12257=CARTESIAN_POINT('Origin',(0.,-2.,0.));
#12258=CARTESIAN_POINT('Origin',(0.115470053837925,-0.5,-0.2));
#12259=CARTESIAN_POINT('',(0.23094010767585,-0.5,0.));
#12260=CARTESIAN_POINT('',(0.115470053837925,-0.5,-0.2));
#12261=CARTESIAN_POINT('',(0.23094010767585,-0.5,0.));
#12262=CARTESIAN_POINT('',(0.115470053837925,-0.8,-0.2));
#12263=CARTESIAN_POINT('',(0.115470053837925,-0.5,-0.2));
#12264=CARTESIAN_POINT('',(0.23094010767585,-0.8,0.));
#12265=CARTESIAN_POINT('',(0.23094010767585,-0.8,0.));
#12266=CARTESIAN_POINT('',(0.23094010767585,-0.5,0.));
#12267=CARTESIAN_POINT('Origin',(-0.115470053837925,-0.5,-0.2));
#12268=CARTESIAN_POINT('',(-0.115470053837925,-0.5,-0.2));
#12269=CARTESIAN_POINT('',(0.115470053837925,-0.5,-0.2));
#12270=CARTESIAN_POINT('',(-0.115470053837925,-0.8,-0.2));
#12271=CARTESIAN_POINT('',(-0.115470053837925,-0.5,-0.2));
#12272=CARTESIAN_POINT('',(0.115470053837925,-0.8,-0.2));
#12273=CARTESIAN_POINT('Origin',(-0.23094010767585,-0.5,-2.77555756156289E-17));
#12274=CARTESIAN_POINT('',(-0.23094010767585,-0.5,-2.82820063659975E-17));
#12275=CARTESIAN_POINT('',(-0.115470053837925,-0.5,-0.2));
#12276=CARTESIAN_POINT('',(-0.23094010767585,-0.8,-2.77555756156289E-17));
#12277=CARTESIAN_POINT('',(-0.23094010767585,-0.5,-2.82820063659975E-17));
#12278=CARTESIAN_POINT('',(-0.115470053837925,-0.8,-0.2));
#12279=CARTESIAN_POINT('Origin',(-0.115470053837925,-0.5,0.2));
#12280=CARTESIAN_POINT('',(-0.115470053837925,-0.5,0.2));
#12281=CARTESIAN_POINT('',(-0.23094010767585,-0.5,-2.82820063659975E-17));
#12282=CARTESIAN_POINT('',(-0.115470053837925,-0.8,0.2));
#12283=CARTESIAN_POINT('',(-0.115470053837925,-0.5,0.2));
#12284=CARTESIAN_POINT('',(-0.23094010767585,-0.8,-2.82820063659975E-17));
#12285=CARTESIAN_POINT('Origin',(0.115470053837925,-0.5,0.2));
#12286=CARTESIAN_POINT('',(0.115470053837925,-0.5,0.2));
#12287=CARTESIAN_POINT('',(-0.115470053837925,-0.5,0.2));
#12288=CARTESIAN_POINT('',(0.115470053837925,-0.8,0.2));
#12289=CARTESIAN_POINT('',(0.115470053837925,-0.5,0.2));
#12290=CARTESIAN_POINT('',(-0.115470053837925,-0.8,0.2));
#12291=CARTESIAN_POINT('Origin',(0.23094010767585,-0.5,0.));
#12292=CARTESIAN_POINT('',(0.115470053837925,-0.5,0.2));
#12293=CARTESIAN_POINT('',(0.115470053837925,-0.8,0.2));
#12294=CARTESIAN_POINT('Origin',(0.,-0.5,0.));
#12295=CARTESIAN_POINT('Origin',(0.,-0.8,0.));
#12296=CARTESIAN_POINT('',(0.,0.,0.));
#12297=CARTESIAN_POINT('Origin',(42.,30.1,5.));
#12298=CARTESIAN_POINT('',(41.725,33.,5.));
#12299=CARTESIAN_POINT('Origin',(42.,33.,5.));
#12300=CARTESIAN_POINT('',(41.725,33.8,5.));
#12301=CARTESIAN_POINT('',(41.725,30.1,5.));
#12302=CARTESIAN_POINT('Origin',(42.,33.8,5.));
#12303=CARTESIAN_POINT('Origin',(39.,30.1,5.));
#12304=CARTESIAN_POINT('',(38.725,33.,5.));
#12305=CARTESIAN_POINT('Origin',(39.,33.,5.));
#12306=CARTESIAN_POINT('',(38.725,33.8,5.));
#12307=CARTESIAN_POINT('',(38.725,30.1,5.));
#12308=CARTESIAN_POINT('Origin',(39.,33.8,5.));
#12309=CARTESIAN_POINT('Origin',(36.,30.1,5.));
#12310=CARTESIAN_POINT('',(35.725,33.,5.));
#12311=CARTESIAN_POINT('Origin',(36.,33.,5.));
#12312=CARTESIAN_POINT('',(35.725,33.8,5.));
#12313=CARTESIAN_POINT('',(35.725,30.1,5.));
#12314=CARTESIAN_POINT('Origin',(36.,33.8,5.));
#12315=CARTESIAN_POINT('Origin',(45.,30.1,5.));
#12316=CARTESIAN_POINT('',(44.725,33.,5.));
#12317=CARTESIAN_POINT('Origin',(45.,33.,5.));
#12318=CARTESIAN_POINT('',(44.725,33.8,5.));
#12319=CARTESIAN_POINT('',(44.725,30.1,5.));
#12320=CARTESIAN_POINT('Origin',(45.,33.8,5.));
#12321=CARTESIAN_POINT('Origin',(46.,33.8,4.));
#12322=CARTESIAN_POINT('',(46.,33.8,4.));
#12323=CARTESIAN_POINT('',(35.,33.8,4.));
#12324=CARTESIAN_POINT('',(46.,33.8,4.));
#12325=CARTESIAN_POINT('',(35.,33.8,6.));
#12326=CARTESIAN_POINT('',(35.,33.8,4.));
#12327=CARTESIAN_POINT('',(46.,33.8,6.));
#12328=CARTESIAN_POINT('',(46.,33.8,6.));
#12329=CARTESIAN_POINT('',(46.,33.8,4.));
#12330=CARTESIAN_POINT('Origin',(46.,33.,4.));
#12331=CARTESIAN_POINT('',(46.,33.,4.));
#12332=CARTESIAN_POINT('',(46.,33.,4.));
#12333=CARTESIAN_POINT('',(46.,33.,6.));
#12334=CARTESIAN_POINT('',(46.,33.,6.));
#12335=CARTESIAN_POINT('',(46.,33.,4.));
#12336=CARTESIAN_POINT('Origin',(35.,33.,4.));
#12337=CARTESIAN_POINT('',(35.,33.,4.));
#12338=CARTESIAN_POINT('',(35.,33.,4.));
#12339=CARTESIAN_POINT('',(35.,33.,6.));
#12340=CARTESIAN_POINT('',(35.,33.,6.));
#12341=CARTESIAN_POINT('',(35.,33.,4.));
#12342=CARTESIAN_POINT('Origin',(35.,33.8,4.));
#12343=CARTESIAN_POINT('',(35.,33.8,4.));
#12344=CARTESIAN_POINT('',(35.,33.8,6.));
#12345=CARTESIAN_POINT('Origin',(40.5,33.4,6.));
#12346=CARTESIAN_POINT('Origin',(40.5,33.4,4.));
#12347=CARTESIAN_POINT('',(0.,0.,0.));
#12348=CARTESIAN_POINT('Origin',(0.,0.09,0.));
#12349=CARTESIAN_POINT('',(-0.285,0.1,3.49024337756996E-17));
#12350=CARTESIAN_POINT('Origin',(0.,0.1,0.));
#12351=CARTESIAN_POINT('',(-0.265,0.08,-3.24531401774049E-17));
#12352=CARTESIAN_POINT('',(-0.275,0.09,3.36777869765522E-17));
#12353=CARTESIAN_POINT('Origin',(0.,0.08,0.));
#12354=CARTESIAN_POINT('Origin',(0.,0.,0.));
#12355=CARTESIAN_POINT('',(-0.265,0.,3.24531401774049E-17));
#12356=CARTESIAN_POINT('',(-0.265,0.,3.24531401774049E-17));
#12357=CARTESIAN_POINT('Origin',(0.,0.,0.));
#12358=CARTESIAN_POINT('Origin',(0.,0.1,0.));
#12359=CARTESIAN_POINT('',(-0.5,0.1,6.12323399573677E-17));
#12360=CARTESIAN_POINT('Origin',(0.,0.1,0.));
#12361=CARTESIAN_POINT('Origin',(0.,0.,0.));
#12362=CARTESIAN_POINT('',(-0.5,0.,6.12323399573677E-17));
#12363=CARTESIAN_POINT('',(-0.5,0.,6.12323399573677E-17));
#12364=CARTESIAN_POINT('Origin',(0.,0.,0.));
#12365=CARTESIAN_POINT('Origin',(0.,0.,0.));
#12366=CARTESIAN_POINT('',(0.,0.,0.));
#12367=CARTESIAN_POINT('Origin',(6.,-2.,-16.9));
#12368=CARTESIAN_POINT('',(5.725,-2.,-16.8));
#12369=CARTESIAN_POINT('Origin',(6.,-2.,-16.8));
#12370=CARTESIAN_POINT('',(5.725,-2.,-16.));
#12371=CARTESIAN_POINT('',(5.725,-2.,-16.9));
#12372=CARTESIAN_POINT('Origin',(6.,-2.,-16.));
#12373=CARTESIAN_POINT('Origin',(6.,32.,-16.9));
#12374=CARTESIAN_POINT('',(5.725,32.,-16.8));
#12375=CARTESIAN_POINT('Origin',(6.,32.,-16.8));
#12376=CARTESIAN_POINT('',(5.725,32.,-16.));
#12377=CARTESIAN_POINT('',(5.725,32.,-16.9));
#12378=CARTESIAN_POINT('Origin',(6.,32.,-16.));
#12379=CARTESIAN_POINT('Origin',(8.,35.,-16.8));
#12380=CARTESIAN_POINT('',(8.,35.,-16.8));
#12381=CARTESIAN_POINT('',(4.,35.,-16.8));
#12382=CARTESIAN_POINT('',(8.,35.,-16.8));
#12383=CARTESIAN_POINT('',(4.,35.,-16.));
#12384=CARTESIAN_POINT('',(4.,35.,-16.8));
#12385=CARTESIAN_POINT('',(8.,35.,-16.));
#12386=CARTESIAN_POINT('',(8.,35.,-16.));
#12387=CARTESIAN_POINT('',(8.,35.,-16.8));
#12388=CARTESIAN_POINT('Origin',(8.,-5.,-16.8));
#12389=CARTESIAN_POINT('',(8.,-5.,-16.8));
#12390=CARTESIAN_POINT('',(8.,-5.,-16.8));
#12391=CARTESIAN_POINT('',(8.,-5.,-16.));
#12392=CARTESIAN_POINT('',(8.,-5.,-16.));
#12393=CARTESIAN_POINT('',(8.,-5.,-16.8));
#12394=CARTESIAN_POINT('Origin',(4.,-5.,-16.8));
#12395=CARTESIAN_POINT('',(4.,-5.,-16.8));
#12396=CARTESIAN_POINT('',(4.,-5.,-16.8));
#12397=CARTESIAN_POINT('',(4.,-5.,-16.));
#12398=CARTESIAN_POINT('',(4.,-5.,-16.));
#12399=CARTESIAN_POINT('',(4.,-5.,-16.8));
#12400=CARTESIAN_POINT('Origin',(4.,35.,-16.8));
#12401=CARTESIAN_POINT('',(4.,35.,-16.8));
#12402=CARTESIAN_POINT('',(4.,35.,-16.));
#12403=CARTESIAN_POINT('Origin',(6.,15.,-16.));
#12404=CARTESIAN_POINT('Origin',(6.,15.,-16.8));
#12405=CARTESIAN_POINT('',(0.,0.,0.));
#12406=CARTESIAN_POINT('Origin',(8.,-3.5,-17.6));
#12407=CARTESIAN_POINT('',(8.,-3.5,-17.6));
#12408=CARTESIAN_POINT('',(4.,-3.5,-17.6));
#12409=CARTESIAN_POINT('',(8.,-3.5,-17.6));
#12410=CARTESIAN_POINT('',(4.,-3.5,-16.8));
#12411=CARTESIAN_POINT('',(4.,-3.5,-17.6));
#12412=CARTESIAN_POINT('',(8.,-3.5,-16.8));
#12413=CARTESIAN_POINT('',(8.,-3.5,-16.8));
#12414=CARTESIAN_POINT('',(8.,-3.5,-17.6));
#12415=CARTESIAN_POINT('Origin',(8.,-5.,-17.6));
#12416=CARTESIAN_POINT('',(8.,-5.,-17.6));
#12417=CARTESIAN_POINT('',(8.,-5.,-17.6));
#12418=CARTESIAN_POINT('',(8.,-5.,-16.8));
#12419=CARTESIAN_POINT('',(8.,-5.,-16.8));
#12420=CARTESIAN_POINT('',(8.,-5.,-17.6));
#12421=CARTESIAN_POINT('Origin',(4.,-5.,-17.6));
#12422=CARTESIAN_POINT('',(4.,-5.,-17.6));
#12423=CARTESIAN_POINT('',(4.,-5.,-17.6));
#12424=CARTESIAN_POINT('',(4.,-5.,-16.8));
#12425=CARTESIAN_POINT('',(4.,-5.,-16.8));
#12426=CARTESIAN_POINT('',(4.,-5.,-17.6));
#12427=CARTESIAN_POINT('Origin',(4.,-3.5,-17.6));
#12428=CARTESIAN_POINT('',(4.,-3.5,-17.6));
#12429=CARTESIAN_POINT('',(4.,-3.5,-16.8));
#12430=CARTESIAN_POINT('Origin',(6.,-4.25,-16.8));
#12431=CARTESIAN_POINT('Origin',(6.,-4.25,-17.6));
#12432=CARTESIAN_POINT('',(0.,0.,0.));
#12433=CARTESIAN_POINT('Origin',(8.,35.,-17.6));
#12434=CARTESIAN_POINT('',(8.,35.,-17.6));
#12435=CARTESIAN_POINT('',(4.,35.,-17.6));
#12436=CARTESIAN_POINT('',(8.,35.,-17.6));
#12437=CARTESIAN_POINT('',(4.,35.,-16.8));
#12438=CARTESIAN_POINT('',(4.,35.,-17.6));
#12439=CARTESIAN_POINT('',(8.,35.,-16.8));
#12440=CARTESIAN_POINT('',(8.,35.,-16.8));
#12441=CARTESIAN_POINT('',(8.,35.,-17.6));
#12442=CARTESIAN_POINT('Origin',(8.,33.5,-17.6));
#12443=CARTESIAN_POINT('',(8.,33.5,-17.6));
#12444=CARTESIAN_POINT('',(8.,33.5,-17.6));
#12445=CARTESIAN_POINT('',(8.,33.5,-16.8));
#12446=CARTESIAN_POINT('',(8.,33.5,-16.8));
#12447=CARTESIAN_POINT('',(8.,33.5,-17.6));
#12448=CARTESIAN_POINT('Origin',(4.,33.5,-17.6));
#12449=CARTESIAN_POINT('',(4.,33.5,-17.6));
#12450=CARTESIAN_POINT('',(4.,33.5,-17.6));
#12451=CARTESIAN_POINT('',(4.,33.5,-16.8));
#12452=CARTESIAN_POINT('',(4.,33.5,-16.8));
#12453=CARTESIAN_POINT('',(4.,33.5,-17.6));
#12454=CARTESIAN_POINT('Origin',(4.,35.,-17.6));
#12455=CARTESIAN_POINT('',(4.,35.,-17.6));
#12456=CARTESIAN_POINT('',(4.,35.,-16.8));
#12457=CARTESIAN_POINT('Origin',(6.,34.25,-16.8));
#12458=CARTESIAN_POINT('Origin',(6.,34.25,-17.6));
#12459=CARTESIAN_POINT('',(0.,0.,0.));
#12460=CARTESIAN_POINT('Origin',(54.,-2.,-16.9));
#12461=CARTESIAN_POINT('',(53.725,-2.,-16.8));
#12462=CARTESIAN_POINT('Origin',(54.,-2.,-16.8));
#12463=CARTESIAN_POINT('',(53.725,-2.,-16.));
#12464=CARTESIAN_POINT('',(53.725,-2.,-16.9));
#12465=CARTESIAN_POINT('Origin',(54.,-2.,-16.));
#12466=CARTESIAN_POINT('Origin',(54.,32.,-16.9));
#12467=CARTESIAN_POINT('',(53.725,32.,-16.8));
#12468=CARTESIAN_POINT('Origin',(54.,32.,-16.8));
#12469=CARTESIAN_POINT('',(53.725,32.,-16.));
#12470=CARTESIAN_POINT('',(53.725,32.,-16.9));
#12471=CARTESIAN_POINT('Origin',(54.,32.,-16.));
#12472=CARTESIAN_POINT('Origin',(56.,35.,-16.8));
#12473=CARTESIAN_POINT('',(56.,35.,-16.8));
#12474=CARTESIAN_POINT('',(52.,35.,-16.8));
#12475=CARTESIAN_POINT('',(56.,35.,-16.8));
#12476=CARTESIAN_POINT('',(52.,35.,-16.));
#12477=CARTESIAN_POINT('',(52.,35.,-16.8));
#12478=CARTESIAN_POINT('',(56.,35.,-16.));
#12479=CARTESIAN_POINT('',(56.,35.,-16.));
#12480=CARTESIAN_POINT('',(56.,35.,-16.8));
#12481=CARTESIAN_POINT('Origin',(56.,-5.,-16.8));
#12482=CARTESIAN_POINT('',(56.,-5.,-16.8));
#12483=CARTESIAN_POINT('',(56.,-5.,-16.8));
#12484=CARTESIAN_POINT('',(56.,-5.,-16.));
#12485=CARTESIAN_POINT('',(56.,-5.,-16.));
#12486=CARTESIAN_POINT('',(56.,-5.,-16.8));
#12487=CARTESIAN_POINT('Origin',(52.,-5.,-16.8));
#12488=CARTESIAN_POINT('',(52.,-5.,-16.8));
#12489=CARTESIAN_POINT('',(52.,-5.,-16.8));
#12490=CARTESIAN_POINT('',(52.,-5.,-16.));
#12491=CARTESIAN_POINT('',(52.,-5.,-16.));
#12492=CARTESIAN_POINT('',(52.,-5.,-16.8));
#12493=CARTESIAN_POINT('Origin',(52.,35.,-16.8));
#12494=CARTESIAN_POINT('',(52.,35.,-16.8));
#12495=CARTESIAN_POINT('',(52.,35.,-16.));
#12496=CARTESIAN_POINT('Origin',(54.,15.,-16.));
#12497=CARTESIAN_POINT('Origin',(54.,15.,-16.8));
#12498=CARTESIAN_POINT('',(0.,0.,0.));
#12499=CARTESIAN_POINT('Origin',(56.,-3.5,-17.6));
#12500=CARTESIAN_POINT('',(56.,-3.5,-17.6));
#12501=CARTESIAN_POINT('',(52.,-3.5,-17.6));
#12502=CARTESIAN_POINT('',(56.,-3.5,-17.6));
#12503=CARTESIAN_POINT('',(52.,-3.5,-16.8));
#12504=CARTESIAN_POINT('',(52.,-3.5,-17.6));
#12505=CARTESIAN_POINT('',(56.,-3.5,-16.8));
#12506=CARTESIAN_POINT('',(56.,-3.5,-16.8));
#12507=CARTESIAN_POINT('',(56.,-3.5,-17.6));
#12508=CARTESIAN_POINT('Origin',(56.,-5.,-17.6));
#12509=CARTESIAN_POINT('',(56.,-5.,-17.6));
#12510=CARTESIAN_POINT('',(56.,-5.,-17.6));
#12511=CARTESIAN_POINT('',(56.,-5.,-16.8));
#12512=CARTESIAN_POINT('',(56.,-5.,-16.8));
#12513=CARTESIAN_POINT('',(56.,-5.,-17.6));
#12514=CARTESIAN_POINT('Origin',(52.,-5.,-17.6));
#12515=CARTESIAN_POINT('',(52.,-5.,-17.6));
#12516=CARTESIAN_POINT('',(52.,-5.,-17.6));
#12517=CARTESIAN_POINT('',(52.,-5.,-16.8));
#12518=CARTESIAN_POINT('',(52.,-5.,-16.8));
#12519=CARTESIAN_POINT('',(52.,-5.,-17.6));
#12520=CARTESIAN_POINT('Origin',(52.,-3.5,-17.6));
#12521=CARTESIAN_POINT('',(52.,-3.5,-17.6));
#12522=CARTESIAN_POINT('',(52.,-3.5,-16.8));
#12523=CARTESIAN_POINT('Origin',(54.,-4.25,-16.8));
#12524=CARTESIAN_POINT('Origin',(54.,-4.25,-17.6));
#12525=CARTESIAN_POINT('',(0.,0.,0.));
#12526=CARTESIAN_POINT('Origin',(56.,35.,-17.6));
#12527=CARTESIAN_POINT('',(56.,35.,-17.6));
#12528=CARTESIAN_POINT('',(52.,35.,-17.6));
#12529=CARTESIAN_POINT('',(56.,35.,-17.6));
#12530=CARTESIAN_POINT('',(52.,35.,-16.8));
#12531=CARTESIAN_POINT('',(52.,35.,-17.6));
#12532=CARTESIAN_POINT('',(56.,35.,-16.8));
#12533=CARTESIAN_POINT('',(56.,35.,-16.8));
#12534=CARTESIAN_POINT('',(56.,35.,-17.6));
#12535=CARTESIAN_POINT('Origin',(56.,33.5,-17.6));
#12536=CARTESIAN_POINT('',(56.,33.5,-17.6));
#12537=CARTESIAN_POINT('',(56.,33.5,-17.6));
#12538=CARTESIAN_POINT('',(56.,33.5,-16.8));
#12539=CARTESIAN_POINT('',(56.,33.5,-16.8));
#12540=CARTESIAN_POINT('',(56.,33.5,-17.6));
#12541=CARTESIAN_POINT('Origin',(52.,33.5,-17.6));
#12542=CARTESIAN_POINT('',(52.,33.5,-17.6));
#12543=CARTESIAN_POINT('',(52.,33.5,-17.6));
#12544=CARTESIAN_POINT('',(52.,33.5,-16.8));
#12545=CARTESIAN_POINT('',(52.,33.5,-16.8));
#12546=CARTESIAN_POINT('',(52.,33.5,-17.6));
#12547=CARTESIAN_POINT('Origin',(52.,35.,-17.6));
#12548=CARTESIAN_POINT('',(52.,35.,-17.6));
#12549=CARTESIAN_POINT('',(52.,35.,-16.8));
#12550=CARTESIAN_POINT('Origin',(54.,34.25,-16.8));
#12551=CARTESIAN_POINT('Origin',(54.,34.25,-17.6));
#12552=CARTESIAN_POINT('',(0.,0.,0.));
#12553=CARTESIAN_POINT('',(0.,0.,0.));
#12554=CARTESIAN_POINT('Origin',(3.,0.,8.));
#12555=CARTESIAN_POINT('',(1.3,30.,8.));
#12556=CARTESIAN_POINT('Origin',(3.,30.,8.));
#12557=CARTESIAN_POINT('',(1.3,0.,8.));
#12558=CARTESIAN_POINT('',(1.3,0.,8.));
#12559=CARTESIAN_POINT('Origin',(3.,0.,8.));
#12560=CARTESIAN_POINT('Origin',(3.,0.,8.));
#12561=CARTESIAN_POINT('',(1.,30.,8.));
#12562=CARTESIAN_POINT('Origin',(3.,30.,8.));
#12563=CARTESIAN_POINT('',(1.,0.,8.));
#12564=CARTESIAN_POINT('',(1.,0.,8.));
#12565=CARTESIAN_POINT('Origin',(3.,0.,8.));
#12566=CARTESIAN_POINT('Origin',(3.,30.,8.));
#12567=CARTESIAN_POINT('Origin',(3.,0.,8.));
#12568=CARTESIAN_POINT('',(0.,0.,0.));
#12569=CARTESIAN_POINT('Origin',(3.,0.95,8.));
#12570=CARTESIAN_POINT('',(1.9,1.2,8.));
#12571=CARTESIAN_POINT('Origin',(3.,1.2,8.));
#12572=CARTESIAN_POINT('',(1.9,0.95,8.));
#12573=CARTESIAN_POINT('',(1.9,0.95,8.));
#12574=CARTESIAN_POINT('Origin',(3.,0.95,8.));
#12575=CARTESIAN_POINT('Origin',(3.,0.95,8.));
#12576=CARTESIAN_POINT('',(1.5,0.95,8.));
#12577=CARTESIAN_POINT('Origin',(3.,0.95,8.));
#12578=CARTESIAN_POINT('Origin',(3.,0.,8.));
#12579=CARTESIAN_POINT('',(1.5,0.,8.));
#12580=CARTESIAN_POINT('',(1.5,0.,8.));
#12581=CARTESIAN_POINT('Origin',(3.,0.,8.));
#12582=CARTESIAN_POINT('Origin',(3.,0.,8.));
#12583=CARTESIAN_POINT('',(1.3,1.2,8.));
#12584=CARTESIAN_POINT('Origin',(3.,1.2,8.));
#12585=CARTESIAN_POINT('',(1.3,0.,8.));
#12586=CARTESIAN_POINT('',(1.3,0.,8.));
#12587=CARTESIAN_POINT('Origin',(3.,0.,8.));
#12588=CARTESIAN_POINT('Origin',(3.,1.2,8.));
#12589=CARTESIAN_POINT('Origin',(3.,0.,8.));
#12590=CARTESIAN_POINT('',(0.,0.,0.));
#12591=CARTESIAN_POINT('Origin',(3.,0.,8.));
#12592=CARTESIAN_POINT('',(1.5,0.,8.));
#12593=CARTESIAN_POINT('Origin',(3.,0.,8.));
#12594=CARTESIAN_POINT('',(1.5,0.05,8.));
#12595=CARTESIAN_POINT('',(1.5,0.,8.));
#12596=CARTESIAN_POINT('Origin',(3.,0.05,8.));
#12597=CARTESIAN_POINT('Origin',(3.,0.05,8.));
#12598=CARTESIAN_POINT('',(1.8,0.05,8.));
#12599=CARTESIAN_POINT('Origin',(3.,0.05,8.));
#12600=CARTESIAN_POINT('Origin',(3.,-0.2,8.));
#12601=CARTESIAN_POINT('',(1.8,-0.2,8.));
#12602=CARTESIAN_POINT('',(1.8,-0.2,8.));
#12603=CARTESIAN_POINT('Origin',(3.,-0.2,8.));
#12604=CARTESIAN_POINT('Origin',(3.,-0.2,8.));
#12605=CARTESIAN_POINT('',(1.,0.,8.));
#12606=CARTESIAN_POINT('Origin',(3.,0.,8.));
#12607=CARTESIAN_POINT('',(1.,-0.2,8.));
#12608=CARTESIAN_POINT('',(1.,-0.2,8.));
#12609=CARTESIAN_POINT('Origin',(3.,-0.2,8.));
#12610=CARTESIAN_POINT('Origin',(3.,0.,8.));
#12611=CARTESIAN_POINT('Origin',(3.,-0.2,8.));
#12612=CARTESIAN_POINT('',(0.,0.,0.));
#12613=CARTESIAN_POINT('Origin',(3.,28.8,8.));
#12614=CARTESIAN_POINT('',(1.9,29.05,8.));
#12615=CARTESIAN_POINT('Origin',(3.,29.05,8.));
#12616=CARTESIAN_POINT('',(1.9,28.8,8.));
#12617=CARTESIAN_POINT('',(1.9,28.8,8.));
#12618=CARTESIAN_POINT('Origin',(3.,28.8,8.));
#12619=CARTESIAN_POINT('Origin',(3.,29.05,8.));
#12620=CARTESIAN_POINT('',(1.5,29.05,8.));
#12621=CARTESIAN_POINT('Origin',(3.,29.05,8.));
#12622=CARTESIAN_POINT('Origin',(3.,28.8,8.));
#12623=CARTESIAN_POINT('',(1.5,30.,8.));
#12624=CARTESIAN_POINT('Origin',(3.,30.,8.));
#12625=CARTESIAN_POINT('',(1.5,28.8,8.));
#12626=CARTESIAN_POINT('Origin',(3.,28.8,8.));
#12627=CARTESIAN_POINT('',(1.3,30.,8.));
#12628=CARTESIAN_POINT('Origin',(3.,30.,8.));
#12629=CARTESIAN_POINT('',(1.3,28.8,8.));
#12630=CARTESIAN_POINT('',(1.3,28.8,8.));
#12631=CARTESIAN_POINT('Origin',(3.,28.8,8.));
#12632=CARTESIAN_POINT('Origin',(3.,30.,8.));
#12633=CARTESIAN_POINT('Origin',(3.,28.8,8.));
#12634=CARTESIAN_POINT('',(0.,0.,0.));
#12635=CARTESIAN_POINT('Origin',(3.,29.95,8.));
#12636=CARTESIAN_POINT('',(1.5,29.95,8.));
#12637=CARTESIAN_POINT('Origin',(3.,29.95,8.));
#12638=CARTESIAN_POINT('',(1.5,30.,8.));
#12639=CARTESIAN_POINT('',(1.5,29.95,8.));
#12640=CARTESIAN_POINT('Origin',(3.,30.,8.));
#12641=CARTESIAN_POINT('Origin',(3.,29.95,8.));
#12642=CARTESIAN_POINT('',(1.8,29.95,8.));
#12643=CARTESIAN_POINT('Origin',(3.,29.95,8.));
#12644=CARTESIAN_POINT('Origin',(3.,30.,8.));
#12645=CARTESIAN_POINT('',(1.8,30.2,8.));
#12646=CARTESIAN_POINT('Origin',(3.,30.2,8.));
#12647=CARTESIAN_POINT('',(1.8,30.,8.));
#12648=CARTESIAN_POINT('Origin',(3.,30.,8.));
#12649=CARTESIAN_POINT('',(1.,30.2,8.));
#12650=CARTESIAN_POINT('Origin',(3.,30.2,8.));
#12651=CARTESIAN_POINT('',(1.,30.,8.));
#12652=CARTESIAN_POINT('',(1.,30.,8.));
#12653=CARTESIAN_POINT('Origin',(3.,30.,8.));
#12654=CARTESIAN_POINT('Origin',(3.,30.2,8.));
#12655=CARTESIAN_POINT('Origin',(3.,30.,8.));
#12656=CARTESIAN_POINT('',(0.,0.,0.));
#12657=CARTESIAN_POINT('Origin',(3.,31.7,8.));
#12658=CARTESIAN_POINT('',(2.835,31.7,8.));
#12659=CARTESIAN_POINT('Origin',(3.,31.7,8.));
#12660=CARTESIAN_POINT('',(2.835,33.,8.));
#12661=CARTESIAN_POINT('',(2.835,31.7,8.));
#12662=CARTESIAN_POINT('Origin',(3.,33.,8.));
#12663=CARTESIAN_POINT('Origin',(3.,31.7,8.));
#12664=CARTESIAN_POINT('Origin',(3.,-3.1,8.));
#12665=CARTESIAN_POINT('',(2.835,-3.,8.));
#12666=CARTESIAN_POINT('Origin',(3.,-3.,8.));
#12667=CARTESIAN_POINT('',(2.835,-1.7,8.));
#12668=CARTESIAN_POINT('',(2.835,-3.1,8.));
#12669=CARTESIAN_POINT('Origin',(3.,-1.7,8.));
#12670=CARTESIAN_POINT('Origin',(3.,-1.7,8.));
#12671=CARTESIAN_POINT('Origin',(3.,-3.,8.));
#12672=CARTESIAN_POINT('',(2.5,33.,8.));
#12673=CARTESIAN_POINT('Origin',(3.,33.,8.));
#12674=CARTESIAN_POINT('',(2.5,-3.,8.));
#12675=CARTESIAN_POINT('',(2.5,-3.,8.));
#12676=CARTESIAN_POINT('Origin',(3.,-3.,8.));
#12677=CARTESIAN_POINT('Origin',(3.,33.,8.));
#12678=CARTESIAN_POINT('Origin',(3.,-3.,8.));
#12679=CARTESIAN_POINT('',(0.,0.,0.));
#12680=CARTESIAN_POINT('Origin',(1.6,-2.,6.9));
#12681=CARTESIAN_POINT('',(1.1,-2.,6.9));
#12682=CARTESIAN_POINT('Origin',(1.6,-2.,6.9));
#12683=CARTESIAN_POINT('',(1.1,-2.,9.));
#12684=CARTESIAN_POINT('',(1.1,-2.,6.9));
#12685=CARTESIAN_POINT('Origin',(1.6,-2.,9.));
#12686=CARTESIAN_POINT('Origin',(1.6,-2.,6.9));
#12687=CARTESIAN_POINT('',(1.325,-2.,6.9));
#12688=CARTESIAN_POINT('Origin',(1.6,-2.,6.9));
#12689=CARTESIAN_POINT('Origin',(4.4,-2.,6.9));
#12690=CARTESIAN_POINT('',(3.9,-2.,6.9));
#12691=CARTESIAN_POINT('Origin',(4.4,-2.,6.9));
#12692=CARTESIAN_POINT('',(3.9,-2.,9.));
#12693=CARTESIAN_POINT('',(3.9,-2.,6.9));
#12694=CARTESIAN_POINT('Origin',(4.4,-2.,9.));
#12695=CARTESIAN_POINT('Origin',(4.4,-2.,6.9));
#12696=CARTESIAN_POINT('',(4.125,-2.,6.9));
#12697=CARTESIAN_POINT('Origin',(4.4,-2.,6.9));
#12698=CARTESIAN_POINT('Origin',(1.6,-2.,5.9));
#12699=CARTESIAN_POINT('',(1.325,-2.,6.));
#12700=CARTESIAN_POINT('Origin',(1.6,-2.,6.));
#12701=CARTESIAN_POINT('',(1.325,-2.,5.9));
#12702=CARTESIAN_POINT('Origin',(4.4,-2.,5.9));
#12703=CARTESIAN_POINT('',(4.125,-2.,6.));
#12704=CARTESIAN_POINT('Origin',(4.4,-2.,6.));
#12705=CARTESIAN_POINT('',(4.125,-2.,5.9));
#12706=CARTESIAN_POINT('Origin',(3.,-3.1,8.));
#12707=CARTESIAN_POINT('',(2.495,-3.,8.));
#12708=CARTESIAN_POINT('Origin',(3.,-3.,8.));
#12709=CARTESIAN_POINT('',(2.495,-1.,8.));
#12710=CARTESIAN_POINT('',(2.495,-3.1,8.));
#12711=CARTESIAN_POINT('Origin',(3.,-1.,8.));
#12712=CARTESIAN_POINT('Origin',(5.,-1.,6.));
#12713=CARTESIAN_POINT('',(5.,-1.,6.));
#12714=CARTESIAN_POINT('',(1.,-1.,6.));
#12715=CARTESIAN_POINT('',(5.,-1.,6.));
#12716=CARTESIAN_POINT('',(1.,-1.,9.));
#12717=CARTESIAN_POINT('',(1.,-1.,6.));
#12718=CARTESIAN_POINT('',(5.,-1.,9.));
#12719=CARTESIAN_POINT('',(5.,-1.,9.));
#12720=CARTESIAN_POINT('',(5.,-1.,6.));
#12721=CARTESIAN_POINT('Origin',(5.,-3.,6.));
#12722=CARTESIAN_POINT('',(5.,-3.,6.));
#12723=CARTESIAN_POINT('',(5.,-3.,6.));
#12724=CARTESIAN_POINT('',(5.,-3.,9.));
#12725=CARTESIAN_POINT('',(5.,-3.,9.));
#12726=CARTESIAN_POINT('',(5.,-3.,6.));
#12727=CARTESIAN_POINT('Origin',(1.,-3.,6.));
#12728=CARTESIAN_POINT('',(1.,-3.,6.));
#12729=CARTESIAN_POINT('',(1.,-3.,6.));
#12730=CARTESIAN_POINT('',(1.,-3.,9.));
#12731=CARTESIAN_POINT('',(1.,-3.,9.));
#12732=CARTESIAN_POINT('',(1.,-3.,6.));
#12733=CARTESIAN_POINT('Origin',(1.,-1.,6.));
#12734=CARTESIAN_POINT('',(1.,-1.,6.));
#12735=CARTESIAN_POINT('',(1.,-1.,9.));
#12736=CARTESIAN_POINT('Origin',(3.,-2.,9.));
#12737=CARTESIAN_POINT('Origin',(3.,-2.,6.));
#12738=CARTESIAN_POINT('',(0.,0.,0.));
#12739=CARTESIAN_POINT('Origin',(3.,-3.2,8.));
#12740=CARTESIAN_POINT('',(2.775,-3.,8.));
#12741=CARTESIAN_POINT('Origin',(3.,-3.,8.));
#12742=CARTESIAN_POINT('',(2.775,-3.2,8.));
#12743=CARTESIAN_POINT('',(2.775,-3.2,8.));
#12744=CARTESIAN_POINT('Origin',(3.,-3.2,8.));
#12745=CARTESIAN_POINT('Origin',(3.,-3.2,8.));
#12746=CARTESIAN_POINT('',(2.3,-3.,8.));
#12747=CARTESIAN_POINT('Origin',(3.,-3.,8.));
#12748=CARTESIAN_POINT('',(2.3,-3.2,8.));
#12749=CARTESIAN_POINT('',(2.3,-3.2,8.));
#12750=CARTESIAN_POINT('Origin',(3.,-3.2,8.));
#12751=CARTESIAN_POINT('Origin',(3.,-3.,8.));
#12752=CARTESIAN_POINT('Origin',(3.,-3.2,8.));
#12753=CARTESIAN_POINT('',(0.,0.,0.));
#12754=CARTESIAN_POINT('Origin',(3.,-1.,8.));
#12755=CARTESIAN_POINT('',(2.495,0.05,8.));
#12756=CARTESIAN_POINT('Origin',(3.,0.05,8.));
#12757=CARTESIAN_POINT('',(2.495,-1.,8.));
#12758=CARTESIAN_POINT('',(2.495,-1.,8.));
#12759=CARTESIAN_POINT('Origin',(3.,-1.,8.));
#12760=CARTESIAN_POINT('Origin',(3.,-1.,8.));
#12761=CARTESIAN_POINT('',(2.3,0.05,8.));
#12762=CARTESIAN_POINT('Origin',(3.,0.05,8.));
#12763=CARTESIAN_POINT('',(2.3,-1.,8.));
#12764=CARTESIAN_POINT('',(2.3,-1.,8.));
#12765=CARTESIAN_POINT('Origin',(3.,-1.,8.));
#12766=CARTESIAN_POINT('Origin',(3.,0.05,8.));
#12767=CARTESIAN_POINT('Origin',(3.,-1.,8.));
#12768=CARTESIAN_POINT('',(0.,0.,0.));
#12769=CARTESIAN_POINT('',(0.,0.,0.));
#12770=CARTESIAN_POINT('Origin',(0.,0.,0.));
#12771=CARTESIAN_POINT('',(-0.976185,-0.246528389340863,-1.19548183562566E-16));
#12772=CARTESIAN_POINT('',(-1.19548183562566E-16,-0.246528389340863,0.976185));
#12773=CARTESIAN_POINT('Origin',(0.,-0.246528389340863,0.));
#12774=CARTESIAN_POINT('Origin',(0.,-0.246528389340863,0.));
#12775=CARTESIAN_POINT('',(-1.19548183562566E-16,0.246528389340863,0.976185));
#12776=CARTESIAN_POINT('Origin',(-1.22464679914735E-16,0.,1.));
#12777=CARTESIAN_POINT('',(-0.976185,0.246528389340863,1.19548183562566E-16));
#12778=CARTESIAN_POINT('Origin',(0.,0.246528389340863,0.));
#12779=CARTESIAN_POINT('Origin',(0.,0.246528389340863,0.));
#12780=CARTESIAN_POINT('Origin',(0.,0.,0.));
#12781=CARTESIAN_POINT('',(-0.976185,0.45,-1.19548183562566E-16));
#12782=CARTESIAN_POINT('',(-0.976185,0.,-1.19548183562566E-16));
#12783=CARTESIAN_POINT('Origin',(0.,0.45,0.));
#12784=CARTESIAN_POINT('Origin',(0.,0.,0.));
#12785=CARTESIAN_POINT('',(-0.5,-0.39,-6.12323399573677E-17));
#12786=CARTESIAN_POINT('Origin',(0.,-0.39,0.));
#12787=CARTESIAN_POINT('',(-0.5,0.39,-6.12323399573677E-17));
#12788=CARTESIAN_POINT('',(-0.5,0.,-6.12323399573677E-17));
#12789=CARTESIAN_POINT('Origin',(0.,0.39,0.));
#12790=CARTESIAN_POINT('Origin',(0.,0.42,0.));
#12791=CARTESIAN_POINT('',(-0.56,0.45,-6.85802207522518E-17));
#12792=CARTESIAN_POINT('',(-0.53,0.42,-6.49062803548097E-17));
#12793=CARTESIAN_POINT('Origin',(0.,0.45,0.));
#12794=CARTESIAN_POINT('Origin',(0.976185,0.45,0.));
#12795=CARTESIAN_POINT('Origin',(0.,0.,0.));
#12796=CARTESIAN_POINT('',(-0.976185,-0.45,-1.19548183562566E-16));
#12797=CARTESIAN_POINT('Origin',(0.,-0.45,0.));
#12798=CARTESIAN_POINT('',(-0.976185,0.,-1.19548183562566E-16));
#12799=CARTESIAN_POINT('Origin',(0.56,-0.45,0.));
#12800=CARTESIAN_POINT('',(-0.56,-0.45,-6.85802207522518E-17));
#12801=CARTESIAN_POINT('Origin',(0.,-0.45,0.));
#12802=CARTESIAN_POINT('Origin',(0.,-0.42,0.));
#12803=CARTESIAN_POINT('',(-0.53,-0.42,-6.49062803548097E-17));
#12804=CARTESIAN_POINT('',(0.,0.,0.));
#12805=CARTESIAN_POINT('Origin',(0.,0.,0.));
#12806=CARTESIAN_POINT('',(-1.023815,0.246528389340863,-1.25381176266905E-16));
#12807=CARTESIAN_POINT('',(-1.25381176266905E-16,0.246528389340863,1.023815));
#12808=CARTESIAN_POINT('Origin',(0.,0.246528389340863,0.));
#12809=CARTESIAN_POINT('Origin',(0.,0.246528389340863,0.));
#12810=CARTESIAN_POINT('',(-1.25381176266905E-16,-0.246528389340863,1.023815));
#12811=CARTESIAN_POINT('Origin',(-1.22464679914735E-16,0.,1.));
#12812=CARTESIAN_POINT('',(-1.023815,-0.246528389340863,1.25381176266905E-16));
#12813=CARTESIAN_POINT('Origin',(0.,-0.246528389340863,0.));
#12814=CARTESIAN_POINT('Origin',(0.,-0.246528389340863,0.));
#12815=CARTESIAN_POINT('Origin',(0.,0.,0.));
#12816=CARTESIAN_POINT('',(-1.023815,-0.45,-1.25381176266905E-16));
#12817=CARTESIAN_POINT('Origin',(0.,-0.45,0.));
#12818=CARTESIAN_POINT('',(-1.023815,0.,-1.25381176266905E-16));
#12819=CARTESIAN_POINT('Origin',(1.44,0.45,0.));
#12820=CARTESIAN_POINT('',(-1.44,0.45,-1.76349139077219E-16));
#12821=CARTESIAN_POINT('Origin',(0.,0.45,0.));
#12822=CARTESIAN_POINT('',(-1.023815,0.45,-1.25381176266905E-16));
#12823=CARTESIAN_POINT('Origin',(0.,0.45,0.));
#12824=CARTESIAN_POINT('Origin',(0.,0.42,0.));
#12825=CARTESIAN_POINT('',(-1.5,0.39,-1.83697019872103E-16));
#12826=CARTESIAN_POINT('Origin',(0.,0.39,0.));
#12827=CARTESIAN_POINT('',(-1.47,0.42,-1.80023079474661E-16));
#12828=CARTESIAN_POINT('Origin',(0.,0.,0.));
#12829=CARTESIAN_POINT('',(-1.5,-0.39,-1.83697019872103E-16));
#12830=CARTESIAN_POINT('Origin',(0.,-0.39,0.));
#12831=CARTESIAN_POINT('',(-1.5,0.,-1.83697019872103E-16));
#12832=CARTESIAN_POINT('Origin',(0.,-0.42,0.));
#12833=CARTESIAN_POINT('',(-1.44,-0.45,-1.76349139077219E-16));
#12834=CARTESIAN_POINT('Origin',(0.,-0.45,0.));
#12835=CARTESIAN_POINT('',(-1.47,-0.42,-1.80023079474661E-16));
#12836=CARTESIAN_POINT('Origin',(1.023815,-0.45,0.));
#12837=CARTESIAN_POINT('Origin',(0.,0.,0.));
#12838=CARTESIAN_POINT('',(-1.023815,0.,-1.25381176266905E-16));
#12839=CARTESIAN_POINT('',(0.,0.,0.));
#12840=CARTESIAN_POINT('Origin',(1.,0.,0.));
#12841=CARTESIAN_POINT('',(1.,-1.78583896120461E-33,0.23815));
#12842=CARTESIAN_POINT('',(1.,-1.78583896120461E-33,-0.23815));
#12843=CARTESIAN_POINT('Origin',(1.,0.,0.));
#12844=CARTESIAN_POINT('Origin',(0.707106781186548,0.,-0.707106781186547));
#12845=CARTESIAN_POINT('',(0.875504261126124,-1.78583896120461E-33,-0.538709301246971));
#12846=CARTESIAN_POINT('',(0.538709301246971,-1.78583896120461E-33,-0.875504261126124));
#12847=CARTESIAN_POINT('Origin',(0.707106781186548,0.,-0.707106781186547));
#12848=CARTESIAN_POINT('Origin',(6.12323399573677E-17,0.,-1.));
#12849=CARTESIAN_POINT('',(0.23815,-1.78583896120461E-33,-1.));
#12850=CARTESIAN_POINT('',(-0.23815,-1.78583896120461E-33,-1.));
#12851=CARTESIAN_POINT('Origin',(6.12323399573677E-17,0.,-1.));
#12852=CARTESIAN_POINT('Origin',(-0.707106781186547,0.,-0.707106781186548));
#12853=CARTESIAN_POINT('',(-0.538709301246971,-1.78583896120461E-33,-0.875504261126124));
#12854=CARTESIAN_POINT('',(-0.875504261126124,-1.78583896120461E-33,-0.538709301246971));
#12855=CARTESIAN_POINT('Origin',(-0.707106781186547,0.,-0.707106781186548));
#12856=CARTESIAN_POINT('Origin',(-1.,0.,-1.22464679914735E-16));
#12857=CARTESIAN_POINT('',(-1.,-1.78583896120461E-33,-0.23815));
#12858=CARTESIAN_POINT('',(-1.,-1.78583896120461E-33,0.23815));
#12859=CARTESIAN_POINT('Origin',(-1.,0.,-1.22464679914735E-16));
#12860=CARTESIAN_POINT('Origin',(-0.707106781186548,0.,0.707106781186547));
#12861=CARTESIAN_POINT('',(-0.875504261126124,-7.94881478324376E-33,0.538709301246971));
#12862=CARTESIAN_POINT('',(-0.538709301246971,4.37713686083455E-33,0.875504261126124));
#12863=CARTESIAN_POINT('Origin',(-0.707106781186548,0.,0.707106781186547));
#12864=CARTESIAN_POINT('Origin',(-1.83697019872103E-16,0.,1.));
#12865=CARTESIAN_POINT('',(-0.23815,-1.78583896120461E-33,1.));
#12866=CARTESIAN_POINT('',(0.23815,-1.78583896120461E-33,1.));
#12867=CARTESIAN_POINT('Origin',(-1.83697019872103E-16,0.,1.));
#12868=CARTESIAN_POINT('Origin',(0.707106781186547,0.,0.707106781186548));
#12869=CARTESIAN_POINT('',(0.538709301246971,-4.86732687222419E-33,0.875504261126124));
#12870=CARTESIAN_POINT('',(0.875504261126124,1.29564894981497E-33,0.538709301246971));
#12871=CARTESIAN_POINT('Origin',(0.707106781186547,0.,0.707106781186548));
#12872=CARTESIAN_POINT('',(0.,0.,0.));
#12873=CARTESIAN_POINT('Origin',(0.707106781186547,0.,0.707106781186548));
#12874=CARTESIAN_POINT('',(0.504455939115715,-0.04763,0.841298510752802));
#12875=CARTESIAN_POINT('',(0.841298510752802,-0.04763,0.504455939115715));
#12876=CARTESIAN_POINT('Ctrl Pts',(0.504455939115715,-0.04763,0.841298510752802));
#12877=CARTESIAN_POINT('Ctrl Pts',(0.508899795931835,-0.0740444353928835,
0.838633903678357));
#12878=CARTESIAN_POINT('Ctrl Pts',(0.517157748491652,-0.0999305678883309,
0.833661031856294));
#12879=CARTESIAN_POINT('Ctrl Pts',(0.537715343527944,-0.142345102874864,
0.820511285096538));
#12880=CARTESIAN_POINT('Ctrl Pts',(0.548874290046456,-0.159766064500479,
0.813159949759));
#12881=CARTESIAN_POINT('Ctrl Pts',(0.573915184558107,-0.190326085855194,
0.795684265985089));
#12882=CARTESIAN_POINT('Ctrl Pts',(0.587792702767295,-0.203463743702801,
0.78555112003688));
#12883=CARTESIAN_POINT('Ctrl Pts',(0.615966552324775,-0.224161999508995,
0.763642258217233));
#12884=CARTESIAN_POINT('Ctrl Pts',(0.631684198665438,-0.232861760990032,
0.750785745543687));
#12885=CARTESIAN_POINT('Ctrl Pts',(0.663382628119203,-0.244251601209411,
0.722929908501543));
#12886=CARTESIAN_POINT('Ctrl Pts',(0.679352081686668,-0.246942143572133,
0.707917883896095));
#12887=CARTESIAN_POINT('Ctrl Pts',(0.707917883896095,-0.246942143572133,
0.679352081686668));
#12888=CARTESIAN_POINT('Ctrl Pts',(0.722929908501543,-0.244251601209411,
0.663382628119203));
#12889=CARTESIAN_POINT('Ctrl Pts',(0.750785745543687,-0.232861760990032,
0.631684198665439));
#12890=CARTESIAN_POINT('Ctrl Pts',(0.763642258217232,-0.224161999508995,
0.615966552324775));
#12891=CARTESIAN_POINT('Ctrl Pts',(0.78555112003688,-0.203463743702801,
0.587792702767295));
#12892=CARTESIAN_POINT('Ctrl Pts',(0.795684265985088,-0.190326085855194,
0.573915184558108));
#12893=CARTESIAN_POINT('Ctrl Pts',(0.813159949759,-0.15976606450048,0.548874290046456));
#12894=CARTESIAN_POINT('Ctrl Pts',(0.820511285096538,-0.142345102874864,
0.537715343527944));
#12895=CARTESIAN_POINT('Ctrl Pts',(0.833661031856294,-0.099930567888331,
0.517157748491653));
#12896=CARTESIAN_POINT('Ctrl Pts',(0.838633903678357,-0.0740444353928835,
0.508899795931835));
#12897=CARTESIAN_POINT('Ctrl Pts',(0.841298510752801,-0.0476299999999999,
0.504455939115715));
#12898=CARTESIAN_POINT('',(0.528110872004958,-0.04763,0.871530771444223));
#12899=CARTESIAN_POINT('Origin',(0.707106781186547,-0.04763,0.707106781186548));
#12900=CARTESIAN_POINT('',(0.871530771444223,-0.04763,0.528110872004959));
#12901=CARTESIAN_POINT('Ctrl Pts',(0.871530771444223,-0.0476300000000001,
0.528110872004958));
#12902=CARTESIAN_POINT('Ctrl Pts',(0.87014664509073,-0.0609922781173483,
0.530395067942936));
#12903=CARTESIAN_POINT('Ctrl Pts',(0.868149331745851,-0.0742967091364493,
0.533674141594226));
#12904=CARTESIAN_POINT('Ctrl Pts',(0.85981294420286,-0.115492077056649,
0.54708917182331));
#12905=CARTESIAN_POINT('Ctrl Pts',(0.850993704737257,-0.141695629206859,
0.560922177770136));
#12906=CARTESIAN_POINT('Ctrl Pts',(0.830754510485543,-0.181890537957859,
0.590422647829571));
#12907=CARTESIAN_POINT('Ctrl Pts',(0.816896541396381,-0.201072148666545,
0.609616703125488));
#12908=CARTESIAN_POINT('Ctrl Pts',(0.792310597819928,-0.223955109275652,
0.641117951819998));
#12909=CARTESIAN_POINT('Ctrl Pts',(0.779109323683612,-0.232742381310829,
0.657208095763053));
#12910=CARTESIAN_POINT('Ctrl Pts',(0.750552691816206,-0.244234834628584,
0.68964083160521));
#12911=CARTESIAN_POINT('Ctrl Pts',(0.735185187071673,-0.246942143572133,
0.705971972091755));
#12912=CARTESIAN_POINT('Ctrl Pts',(0.705971972091754,-0.246942143572133,
0.735185187071673));
#12913=CARTESIAN_POINT('Ctrl Pts',(0.689640831605209,-0.244234834628584,
0.750552691816206));
#12914=CARTESIAN_POINT('Ctrl Pts',(0.657208095763052,-0.232742381310829,
0.779109323683612));
#12915=CARTESIAN_POINT('Ctrl Pts',(0.641117951819998,-0.223955109275652,
0.792310597819928));
#12916=CARTESIAN_POINT('Ctrl Pts',(0.609616703125487,-0.201072148666545,
0.816896541396382));
#12917=CARTESIAN_POINT('Ctrl Pts',(0.590422647829571,-0.181890537957858,
0.830754510485544));
#12918=CARTESIAN_POINT('Ctrl Pts',(0.560922177770135,-0.141695629206858,
0.850993704737257));
#12919=CARTESIAN_POINT('Ctrl Pts',(0.547089171823309,-0.115492077056649,
0.859812944202861));
#12920=CARTESIAN_POINT('Ctrl Pts',(0.533674141594226,-0.0742967091364491,
0.868149331745852));
#12921=CARTESIAN_POINT('Ctrl Pts',(0.530395067942936,-0.0609922781173483,
0.870146645090731));
#12922=CARTESIAN_POINT('Ctrl Pts',(0.528110872004958,-0.0476300000000001,
0.871530771444223));
#12923=CARTESIAN_POINT('Origin',(0.707106781186547,-0.04763,0.707106781186548));
#12924=CARTESIAN_POINT('Origin',(0.,-0.166705,0.));
#12925=CARTESIAN_POINT('',(0.242834539687906,-0.04763,0.989696097314));
#12926=CARTESIAN_POINT('Origin',(0.,-0.04763,0.));
#12927=CARTESIAN_POINT('',(-0.242834539687907,-0.04763,0.989696097314));
#12928=CARTESIAN_POINT('Ctrl Pts',(0.242834539687906,-0.04763,0.989696097314));
#12929=CARTESIAN_POINT('Ctrl Pts',(0.24024064412003,-0.0609922781173483,
0.990332542620729));
#12930=CARTESIAN_POINT('Ctrl Pts',(0.236509675094874,-0.0742967091364492,
0.991238884025248));
#12931=CARTESIAN_POINT('Ctrl Pts',(0.221129100087819,-0.115492077056649,
0.994830026707808));
#12932=CARTESIAN_POINT('Ctrl Pts',(0.205111543747588,-0.141695629206859,
0.998375294985966));
#12933=CARTESIAN_POINT('Ctrl Pts',(0.169940289819232,-0.181890537957859,
1.00492400591205));
#12934=CARTESIAN_POINT('Ctrl Pts',(0.1465689792446,-0.201072148666545,1.00869718865384));
#12935=CARTESIAN_POINT('Ctrl Pts',(0.106909345252087,-0.223955109275652,
1.01358704779679));
#12936=CARTESIAN_POINT('Ctrl Pts',(0.0861971848975941,-0.232742381310829,
1.0156297872271));
#12937=CARTESIAN_POINT('Ctrl Pts',(0.0430711894098822,-0.244234834628584,
1.01837060663223));
#12938=CARTESIAN_POINT('Ctrl Pts',(0.0206568624125605,-0.246942143572133,
1.019052));
#12939=CARTESIAN_POINT('Ctrl Pts',(-0.0206568624125608,-0.246942143572133,
1.019052));
#12940=CARTESIAN_POINT('Ctrl Pts',(-0.0430711894098825,-0.244234834628584,
1.01837060663223));
#12941=CARTESIAN_POINT('Ctrl Pts',(-0.0861971848975943,-0.232742381310829,
1.0156297872271));
#12942=CARTESIAN_POINT('Ctrl Pts',(-0.106909345252088,-0.223955109275652,
1.01358704779679));
#12943=CARTESIAN_POINT('Ctrl Pts',(-0.1465689792446,-0.201072148666545,
1.00869718865384));
#12944=CARTESIAN_POINT('Ctrl Pts',(-0.169940289819232,-0.181890537957859,
1.00492400591205));
#12945=CARTESIAN_POINT('Ctrl Pts',(-0.205111543747588,-0.141695629206859,
0.998375294985966));
#12946=CARTESIAN_POINT('Ctrl Pts',(-0.221129100087819,-0.115492077056649,
0.994830026707808));
#12947=CARTESIAN_POINT('Ctrl Pts',(-0.236509675094875,-0.0742967091364493,
0.991238884025248));
#12948=CARTESIAN_POINT('Ctrl Pts',(-0.24024064412003,-0.0609922781173483,
0.990332542620729));
#12949=CARTESIAN_POINT('Ctrl Pts',(-0.242834539687907,-0.04763,0.989696097314));
#12950=CARTESIAN_POINT('',(-0.528110872004959,-0.04763,0.871530771444223));
#12951=CARTESIAN_POINT('Origin',(0.,-0.04763,0.));
#12952=CARTESIAN_POINT('',(-0.871530771444223,-0.04763,0.528110872004958));
#12953=CARTESIAN_POINT('Ctrl Pts',(-0.528110872004958,-0.0476300000000001,
0.871530771444223));
#12954=CARTESIAN_POINT('Ctrl Pts',(-0.530395067942936,-0.0609922781173484,
0.87014664509073));
#12955=CARTESIAN_POINT('Ctrl Pts',(-0.533674141594226,-0.0742967091364493,
0.868149331745851));
#12956=CARTESIAN_POINT('Ctrl Pts',(-0.54708917182331,-0.115492077056649,
0.85981294420286));
#12957=CARTESIAN_POINT('Ctrl Pts',(-0.560922177770136,-0.141695629206859,
0.850993704737257));
#12958=CARTESIAN_POINT('Ctrl Pts',(-0.590422647829571,-0.181890537957859,
0.830754510485543));
#12959=CARTESIAN_POINT('Ctrl Pts',(-0.609616703125488,-0.201072148666545,
0.816896541396381));
#12960=CARTESIAN_POINT('Ctrl Pts',(-0.641117951819998,-0.223955109275652,
0.792310597819928));
#12961=CARTESIAN_POINT('Ctrl Pts',(-0.657208095763053,-0.232742381310829,
0.779109323683611));
#12962=CARTESIAN_POINT('Ctrl Pts',(-0.68964083160521,-0.244234834628584,
0.750552691816205));
#12963=CARTESIAN_POINT('Ctrl Pts',(-0.705971972091755,-0.246942143572133,
0.735185187071673));
#12964=CARTESIAN_POINT('Ctrl Pts',(-0.735185187071673,-0.246942143572133,
0.705971972091754));
#12965=CARTESIAN_POINT('Ctrl Pts',(-0.750552691816206,-0.244234834628584,
0.689640831605209));
#12966=CARTESIAN_POINT('Ctrl Pts',(-0.779109323683612,-0.232742381310829,
0.657208095763052));
#12967=CARTESIAN_POINT('Ctrl Pts',(-0.792310597819928,-0.223955109275652,
0.641117951819998));
#12968=CARTESIAN_POINT('Ctrl Pts',(-0.816896541396382,-0.201072148666545,
0.609616703125487));
#12969=CARTESIAN_POINT('Ctrl Pts',(-0.830754510485544,-0.181890537957858,
0.590422647829571));
#12970=CARTESIAN_POINT('Ctrl Pts',(-0.850993704737257,-0.141695629206858,
0.560922177770135));
#12971=CARTESIAN_POINT('Ctrl Pts',(-0.859812944202861,-0.115492077056649,
0.547089171823309));
#12972=CARTESIAN_POINT('Ctrl Pts',(-0.868149331745852,-0.0742967091364491,
0.533674141594226));
#12973=CARTESIAN_POINT('Ctrl Pts',(-0.870146645090731,-0.0609922781173483,
0.530395067942936));
#12974=CARTESIAN_POINT('Ctrl Pts',(-0.871530771444223,-0.04763,0.528110872004958));
#12975=CARTESIAN_POINT('',(-0.989696097314,-0.04763,0.242834539687906));
#12976=CARTESIAN_POINT('Origin',(0.,-0.04763,0.));
#12977=CARTESIAN_POINT('',(-1.019052,-0.246942143572133,1.248489836334E-16));
#12978=CARTESIAN_POINT('Ctrl Pts',(-0.989696097314,-0.04763,0.242834539687906));
#12979=CARTESIAN_POINT('Ctrl Pts',(-0.990332542620729,-0.0609922781173483,
0.24024064412003));
#12980=CARTESIAN_POINT('Ctrl Pts',(-0.991238884025248,-0.0742967091364492,
0.236509675094874));
#12981=CARTESIAN_POINT('Ctrl Pts',(-0.994830026707808,-0.115492077056649,
0.221129100087819));
#12982=CARTESIAN_POINT('Ctrl Pts',(-0.998375294985966,-0.141695629206859,
0.205111543747588));
#12983=CARTESIAN_POINT('Ctrl Pts',(-1.00492400591205,-0.181890537957859,
0.169940289819232));
#12984=CARTESIAN_POINT('Ctrl Pts',(-1.00869718865384,-0.201072148666545,
0.1465689792446));
#12985=CARTESIAN_POINT('Ctrl Pts',(-1.01358704779679,-0.223955109275652,
0.106909345252088));
#12986=CARTESIAN_POINT('Ctrl Pts',(-1.0156297872271,-0.232742381310829,
0.0861971848975944));
#12987=CARTESIAN_POINT('Ctrl Pts',(-1.01837060663223,-0.244234834628584,
0.0430711894098825));
#12988=CARTESIAN_POINT('Ctrl Pts',(-1.019052,-0.246942143572133,0.0206568624125608));
#12989=CARTESIAN_POINT('Ctrl Pts',(-1.019052,-0.246942143572133,1.2490009027033E-16));
#12990=CARTESIAN_POINT('',(-1.019052,-0.28578,1.24797876996471E-16));
#12991=CARTESIAN_POINT('',(-1.019052,-0.166705,1.24797876996471E-16));
#12992=CARTESIAN_POINT('Origin',(0.,-0.28578,0.));
#12993=CARTESIAN_POINT('',(-0.989696097314,-0.04763,-0.242834539687906));
#12994=CARTESIAN_POINT('Ctrl Pts',(-1.019052,-0.246942143572133,1.2490009027033E-16));
#12995=CARTESIAN_POINT('Ctrl Pts',(-1.019052,-0.246942143572133,-0.0206568624125605));
#12996=CARTESIAN_POINT('Ctrl Pts',(-1.01837060663223,-0.244234834628584,
-0.0430711894098822));
#12997=CARTESIAN_POINT('Ctrl Pts',(-1.0156297872271,-0.232742381310829,
-0.0861971848975941));
#12998=CARTESIAN_POINT('Ctrl Pts',(-1.01358704779679,-0.223955109275652,
-0.106909345252087));
#12999=CARTESIAN_POINT('Ctrl Pts',(-1.00869718865384,-0.201072148666546,
-0.1465689792446));
#13000=CARTESIAN_POINT('Ctrl Pts',(-1.00492400591205,-0.181890537957859,
-0.169940289819232));
#13001=CARTESIAN_POINT('Ctrl Pts',(-0.998375294985966,-0.141695629206859,
-0.205111543747588));
#13002=CARTESIAN_POINT('Ctrl Pts',(-0.994830026707808,-0.11549207705665,
-0.221129100087819));
#13003=CARTESIAN_POINT('Ctrl Pts',(-0.991238884025248,-0.0742967091364495,
-0.236509675094874));
#13004=CARTESIAN_POINT('Ctrl Pts',(-0.990332542620729,-0.0609922781173484,
-0.24024064412003));
#13005=CARTESIAN_POINT('Ctrl Pts',(-0.989696097314,-0.0476300000000001,
-0.242834539687907));
#13006=CARTESIAN_POINT('',(-0.871530771444223,-0.04763,-0.528110872004958));
#13007=CARTESIAN_POINT('Origin',(0.,-0.04763,0.));
#13008=CARTESIAN_POINT('',(-0.528110872004958,-0.04763,-0.871530771444223));
#13009=CARTESIAN_POINT('Ctrl Pts',(-0.871530771444223,-0.0476300000000001,
-0.528110872004958));
#13010=CARTESIAN_POINT('Ctrl Pts',(-0.87014664509073,-0.0609922781173484,
-0.530395067942936));
#13011=CARTESIAN_POINT('Ctrl Pts',(-0.868149331745851,-0.0742967091364494,
-0.533674141594226));
#13012=CARTESIAN_POINT('Ctrl Pts',(-0.85981294420286,-0.115492077056649,
-0.54708917182331));
#13013=CARTESIAN_POINT('Ctrl Pts',(-0.850993704737257,-0.141695629206859,
-0.560922177770136));
#13014=CARTESIAN_POINT('Ctrl Pts',(-0.830754510485543,-0.181890537957859,
-0.590422647829571));
#13015=CARTESIAN_POINT('Ctrl Pts',(-0.816896541396381,-0.201072148666546,
-0.609616703125488));
#13016=CARTESIAN_POINT('Ctrl Pts',(-0.792310597819928,-0.223955109275652,
-0.641117951819999));
#13017=CARTESIAN_POINT('Ctrl Pts',(-0.779109323683611,-0.232742381310829,
-0.657208095763053));
#13018=CARTESIAN_POINT('Ctrl Pts',(-0.750552691816205,-0.244234834628584,
-0.68964083160521));
#13019=CARTESIAN_POINT('Ctrl Pts',(-0.735185187071673,-0.246942143572133,
-0.705971972091755));
#13020=CARTESIAN_POINT('Ctrl Pts',(-0.705971972091754,-0.246942143572133,
-0.735185187071673));
#13021=CARTESIAN_POINT('Ctrl Pts',(-0.68964083160521,-0.244234834628584,
-0.750552691816206));
#13022=CARTESIAN_POINT('Ctrl Pts',(-0.657208095763052,-0.232742381310829,
-0.779109323683612));
#13023=CARTESIAN_POINT('Ctrl Pts',(-0.641117951819998,-0.223955109275652,
-0.792310597819928));
#13024=CARTESIAN_POINT('Ctrl Pts',(-0.609616703125488,-0.201072148666545,
-0.816896541396381));
#13025=CARTESIAN_POINT('Ctrl Pts',(-0.590422647829571,-0.181890537957859,
-0.830754510485543));
#13026=CARTESIAN_POINT('Ctrl Pts',(-0.560922177770136,-0.141695629206859,
-0.850993704737257));
#13027=CARTESIAN_POINT('Ctrl Pts',(-0.54708917182331,-0.115492077056649,
-0.85981294420286));
#13028=CARTESIAN_POINT('Ctrl Pts',(-0.533674141594226,-0.0742967091364494,
-0.868149331745852));
#13029=CARTESIAN_POINT('Ctrl Pts',(-0.530395067942936,-0.0609922781173484,
-0.870146645090731));
#13030=CARTESIAN_POINT('Ctrl Pts',(-0.528110872004958,-0.0476300000000001,
-0.871530771444223));
#13031=CARTESIAN_POINT('',(-0.242834539687906,-0.04763,-0.989696097314));
#13032=CARTESIAN_POINT('Origin',(0.,-0.04763,0.));
#13033=CARTESIAN_POINT('',(0.242834539687906,-0.04763,-0.989696097314));
#13034=CARTESIAN_POINT('Ctrl Pts',(-0.242834539687907,-0.04763,-0.989696097314));
#13035=CARTESIAN_POINT('Ctrl Pts',(-0.24024064412003,-0.0609922781173483,
-0.990332542620729));
#13036=CARTESIAN_POINT('Ctrl Pts',(-0.236509675094874,-0.0742967091364493,
-0.991238884025248));
#13037=CARTESIAN_POINT('Ctrl Pts',(-0.221129100087819,-0.115492077056649,
-0.994830026707808));
#13038=CARTESIAN_POINT('Ctrl Pts',(-0.205111543747588,-0.141695629206859,
-0.998375294985966));
#13039=CARTESIAN_POINT('Ctrl Pts',(-0.169940289819232,-0.181890537957859,
-1.00492400591205));
#13040=CARTESIAN_POINT('Ctrl Pts',(-0.1465689792446,-0.201072148666545,
-1.00869718865384));
#13041=CARTESIAN_POINT('Ctrl Pts',(-0.106909345252087,-0.223955109275652,
-1.01358704779679));
#13042=CARTESIAN_POINT('Ctrl Pts',(-0.0861971848975942,-0.232742381310829,
-1.0156297872271));
#13043=CARTESIAN_POINT('Ctrl Pts',(-0.0430711894098823,-0.244234834628584,
-1.01837060663223));
#13044=CARTESIAN_POINT('Ctrl Pts',(-0.0206568624125606,-0.246942143572133,
-1.019052));
#13045=CARTESIAN_POINT('Ctrl Pts',(0.0206568624125607,-0.246942143572133,
-1.019052));
#13046=CARTESIAN_POINT('Ctrl Pts',(0.0430711894098824,-0.244234834628584,
-1.01837060663223));
#13047=CARTESIAN_POINT('Ctrl Pts',(0.0861971848975943,-0.232742381310829,
-1.0156297872271));
#13048=CARTESIAN_POINT('Ctrl Pts',(0.106909345252088,-0.223955109275652,
-1.01358704779679));
#13049=CARTESIAN_POINT('Ctrl Pts',(0.1465689792446,-0.201072148666545,-1.00869718865384));
#13050=CARTESIAN_POINT('Ctrl Pts',(0.169940289819232,-0.181890537957859,
-1.00492400591205));
#13051=CARTESIAN_POINT('Ctrl Pts',(0.205111543747588,-0.141695629206859,
-0.998375294985966));
#13052=CARTESIAN_POINT('Ctrl Pts',(0.221129100087819,-0.115492077056649,
-0.994830026707808));
#13053=CARTESIAN_POINT('Ctrl Pts',(0.236509675094874,-0.0742967091364493,
-0.991238884025248));
#13054=CARTESIAN_POINT('Ctrl Pts',(0.24024064412003,-0.0609922781173484,
-0.990332542620729));
#13055=CARTESIAN_POINT('Ctrl Pts',(0.242834539687907,-0.04763,-0.989696097314));
#13056=CARTESIAN_POINT('',(0.528110872004958,-0.04763,-0.871530771444223));
#13057=CARTESIAN_POINT('Origin',(0.,-0.04763,0.));
#13058=CARTESIAN_POINT('',(0.871530771444223,-0.04763,-0.528110872004958));
#13059=CARTESIAN_POINT('Ctrl Pts',(0.528110872004958,-0.0476300000000001,
-0.871530771444223));
#13060=CARTESIAN_POINT('Ctrl Pts',(0.530395067942936,-0.0609922781173484,
-0.870146645090731));
#13061=CARTESIAN_POINT('Ctrl Pts',(0.533674141594226,-0.0742967091364493,
-0.868149331745851));
#13062=CARTESIAN_POINT('Ctrl Pts',(0.54708917182331,-0.115492077056649,
-0.85981294420286));
#13063=CARTESIAN_POINT('Ctrl Pts',(0.560922177770136,-0.141695629206859,
-0.850993704737257));
#13064=CARTESIAN_POINT('Ctrl Pts',(0.590422647829571,-0.181890537957859,
-0.830754510485543));
#13065=CARTESIAN_POINT('Ctrl Pts',(0.609616703125488,-0.201072148666545,
-0.816896541396381));
#13066=CARTESIAN_POINT('Ctrl Pts',(0.641117951819998,-0.223955109275652,
-0.792310597819928));
#13067=CARTESIAN_POINT('Ctrl Pts',(0.657208095763053,-0.232742381310829,
-0.779109323683612));
#13068=CARTESIAN_POINT('Ctrl Pts',(0.68964083160521,-0.244234834628584,
-0.750552691816206));
#13069=CARTESIAN_POINT('Ctrl Pts',(0.705971972091755,-0.246942143572133,
-0.735185187071673));
#13070=CARTESIAN_POINT('Ctrl Pts',(0.735185187071673,-0.246942143572133,
-0.705971972091754));
#13071=CARTESIAN_POINT('Ctrl Pts',(0.750552691816206,-0.244234834628584,
-0.68964083160521));
#13072=CARTESIAN_POINT('Ctrl Pts',(0.779109323683612,-0.232742381310829,
-0.657208095763053));
#13073=CARTESIAN_POINT('Ctrl Pts',(0.792310597819928,-0.223955109275652,
-0.641117951819998));
#13074=CARTESIAN_POINT('Ctrl Pts',(0.816896541396381,-0.201072148666545,
-0.609616703125488));
#13075=CARTESIAN_POINT('Ctrl Pts',(0.830754510485543,-0.181890537957859,
-0.590422647829571));
#13076=CARTESIAN_POINT('Ctrl Pts',(0.850993704737257,-0.141695629206859,
-0.560922177770136));
#13077=CARTESIAN_POINT('Ctrl Pts',(0.85981294420286,-0.115492077056649,
-0.54708917182331));
#13078=CARTESIAN_POINT('Ctrl Pts',(0.868149331745851,-0.0742967091364493,
-0.533674141594226));
#13079=CARTESIAN_POINT('Ctrl Pts',(0.870146645090731,-0.0609922781173484,
-0.530395067942936));
#13080=CARTESIAN_POINT('Ctrl Pts',(0.871530771444223,-0.0476300000000001,
-0.528110872004958));
#13081=CARTESIAN_POINT('',(0.989696097314,-0.04763,-0.242834539687906));
#13082=CARTESIAN_POINT('Origin',(0.,-0.04763,0.));
#13083=CARTESIAN_POINT('',(0.989696097314,-0.04763,0.242834539687906));
#13084=CARTESIAN_POINT('Ctrl Pts',(0.989696097314,-0.04763,-0.242834539687907));
#13085=CARTESIAN_POINT('Ctrl Pts',(0.990332542620729,-0.0609922781173483,
-0.24024064412003));
#13086=CARTESIAN_POINT('Ctrl Pts',(0.991238884025248,-0.0742967091364493,
-0.236509675094874));
#13087=CARTESIAN_POINT('Ctrl Pts',(0.994830026707808,-0.115492077056649,
-0.221129100087819));
#13088=CARTESIAN_POINT('Ctrl Pts',(0.998375294985966,-0.141695629206859,
-0.205111543747588));
#13089=CARTESIAN_POINT('Ctrl Pts',(1.00492400591205,-0.181890537957859,
-0.169940289819232));
#13090=CARTESIAN_POINT('Ctrl Pts',(1.00869718865384,-0.201072148666545,
-0.1465689792446));
#13091=CARTESIAN_POINT('Ctrl Pts',(1.01358704779679,-0.223955109275652,
-0.106909345252087));
#13092=CARTESIAN_POINT('Ctrl Pts',(1.0156297872271,-0.232742381310829,-0.0861971848975942));
#13093=CARTESIAN_POINT('Ctrl Pts',(1.01837060663223,-0.244234834628584,
-0.0430711894098823));
#13094=CARTESIAN_POINT('Ctrl Pts',(1.019052,-0.246942143572133,-0.0206568624125607));
#13095=CARTESIAN_POINT('Ctrl Pts',(1.019052,-0.246942143572133,0.0206568624125607));
#13096=CARTESIAN_POINT('Ctrl Pts',(1.01837060663223,-0.244234834628584,
0.0430711894098823));
#13097=CARTESIAN_POINT('Ctrl Pts',(1.0156297872271,-0.232742381310829,0.0861971848975942));
#13098=CARTESIAN_POINT('Ctrl Pts',(1.01358704779679,-0.223955109275652,
0.106909345252087));
#13099=CARTESIAN_POINT('Ctrl Pts',(1.00869718865384,-0.201072148666545,
0.1465689792446));
#13100=CARTESIAN_POINT('Ctrl Pts',(1.00492400591205,-0.181890537957859,
0.169940289819232));
#13101=CARTESIAN_POINT('Ctrl Pts',(0.998375294985966,-0.141695629206859,
0.205111543747588));
#13102=CARTESIAN_POINT('Ctrl Pts',(0.994830026707808,-0.115492077056649,
0.221129100087819));
#13103=CARTESIAN_POINT('Ctrl Pts',(0.991238884025248,-0.0742967091364492,
0.236509675094874));
#13104=CARTESIAN_POINT('Ctrl Pts',(0.990332542620729,-0.0609922781173483,
0.24024064412003));
#13105=CARTESIAN_POINT('Ctrl Pts',(0.989696097314,-0.04763,0.242834539687907));
#13106=CARTESIAN_POINT('Origin',(0.,-0.04763,0.));
#13107=CARTESIAN_POINT('Origin',(0.,-0.04763,0.));
#13108=CARTESIAN_POINT('',(0.238183666596899,-0.04763,0.951592097314));
#13109=CARTESIAN_POINT('Origin',(0.,-0.04763,0.));
#13110=CARTESIAN_POINT('Origin',(-1.94289029309402E-16,-0.04763,1.));
#13111=CARTESIAN_POINT('Origin',(-1.94289029309402E-16,0.,1.));
#13112=CARTESIAN_POINT('',(-0.2381836665969,-0.04763,0.951592097314));
#13113=CARTESIAN_POINT('Ctrl Pts',(-0.238183666596899,-0.0476299999999999,
0.951592097314));
#13114=CARTESIAN_POINT('Ctrl Pts',(-0.233157223576062,-0.0740444353928835,
0.952850216871763));
#13115=CARTESIAN_POINT('Ctrl Pts',(-0.223801617934946,-0.0999305678883309,
0.955173119738174));
#13116=CARTESIAN_POINT('Ctrl Pts',(-0.199966927975188,-0.142345102874864,
0.960411259488514));
#13117=CARTESIAN_POINT('Ctrl Pts',(-0.1868781821531,-0.159766064500479,
0.963103647174702));
#13118=CARTESIAN_POINT('Ctrl Pts',(-0.15681442133453,-0.190326085855194,
0.968453058988463));
#13119=CARTESIAN_POINT('Ctrl Pts',(-0.139836317888043,-0.203463743702801,
0.971100730005489));
#13120=CARTESIAN_POINT('Ctrl Pts',(-0.104422493053067,-0.224161999508995,
0.975530745318961));
#13121=CARTESIAN_POINT('Ctrl Pts',(-0.0842175114474176,-0.232861760990032,
0.977553872336861));
#13122=CARTESIAN_POINT('Ctrl Pts',(-0.0421062857595701,-0.244251601209411,
0.980270995488453));
#13123=CARTESIAN_POINT('Ctrl Pts',(-0.0201990724523197,-0.246942143572133,
0.980948));
#13124=CARTESIAN_POINT('Ctrl Pts',(0.020199072452319,-0.246942143572133,
0.980948));
#13125=CARTESIAN_POINT('Ctrl Pts',(0.0421062857595694,-0.244251601209411,
0.980270995488454));
#13126=CARTESIAN_POINT('Ctrl Pts',(0.0842175114474169,-0.232861760990032,
0.977553872336861));
#13127=CARTESIAN_POINT('Ctrl Pts',(0.104422493053067,-0.224161999508995,
0.975530745318961));
#13128=CARTESIAN_POINT('Ctrl Pts',(0.139836317888042,-0.203463743702801,
0.971100730005489));
#13129=CARTESIAN_POINT('Ctrl Pts',(0.15681442133453,-0.190326085855194,
0.968453058988463));
#13130=CARTESIAN_POINT('Ctrl Pts',(0.1868781821531,-0.15976606450048,0.963103647174702));
#13131=CARTESIAN_POINT('Ctrl Pts',(0.199966927975188,-0.142345102874864,
0.960411259488514));
#13132=CARTESIAN_POINT('Ctrl Pts',(0.223801617934945,-0.0999305678883309,
0.955173119738174));
#13133=CARTESIAN_POINT('Ctrl Pts',(0.233157223576061,-0.0740444353928835,
0.952850216871763));
#13134=CARTESIAN_POINT('Ctrl Pts',(0.238183666596899,-0.0476299999999999,
0.951592097314));
#13135=CARTESIAN_POINT('Origin',(-1.94289029309402E-16,-0.04763,1.));
#13136=CARTESIAN_POINT('Origin',(0.,-0.04763,0.));
#13137=CARTESIAN_POINT('',(-0.504455939115715,-0.04763,0.841298510752802));
#13138=CARTESIAN_POINT('Origin',(0.,-0.04763,0.));
#13139=CARTESIAN_POINT('Origin',(-0.707106781186548,-0.04763,0.707106781186547));
#13140=CARTESIAN_POINT('Origin',(-0.707106781186548,0.,0.707106781186547));
#13141=CARTESIAN_POINT('',(-0.841298510752802,-0.04763,0.504455939115715));
#13142=CARTESIAN_POINT('Ctrl Pts',(-0.841298510752802,-0.04763,0.504455939115715));
#13143=CARTESIAN_POINT('Ctrl Pts',(-0.838633903678357,-0.0740444353928835,
0.508899795931835));
#13144=CARTESIAN_POINT('Ctrl Pts',(-0.833661031856294,-0.0999305678883309,
0.517157748491652));
#13145=CARTESIAN_POINT('Ctrl Pts',(-0.820511285096538,-0.142345102874864,
0.537715343527944));
#13146=CARTESIAN_POINT('Ctrl Pts',(-0.813159949759,-0.159766064500479,0.548874290046456));
#13147=CARTESIAN_POINT('Ctrl Pts',(-0.795684265985089,-0.190326085855194,
0.573915184558107));
#13148=CARTESIAN_POINT('Ctrl Pts',(-0.78555112003688,-0.203463743702801,
0.587792702767295));
#13149=CARTESIAN_POINT('Ctrl Pts',(-0.763642258217233,-0.224161999508995,
0.615966552324775));
#13150=CARTESIAN_POINT('Ctrl Pts',(-0.750785745543687,-0.232861760990032,
0.631684198665438));
#13151=CARTESIAN_POINT('Ctrl Pts',(-0.722929908501543,-0.244251601209411,
0.663382628119203));
#13152=CARTESIAN_POINT('Ctrl Pts',(-0.707917883896095,-0.246942143572133,
0.679352081686668));
#13153=CARTESIAN_POINT('Ctrl Pts',(-0.679352081686668,-0.246942143572133,
0.707917883896095));
#13154=CARTESIAN_POINT('Ctrl Pts',(-0.663382628119203,-0.244251601209411,
0.722929908501544));
#13155=CARTESIAN_POINT('Ctrl Pts',(-0.631684198665438,-0.232861760990031,
0.750785745543687));
#13156=CARTESIAN_POINT('Ctrl Pts',(-0.615966552324775,-0.224161999508995,
0.763642258217233));
#13157=CARTESIAN_POINT('Ctrl Pts',(-0.587792702767295,-0.203463743702801,
0.78555112003688));
#13158=CARTESIAN_POINT('Ctrl Pts',(-0.573915184558107,-0.190326085855194,
0.795684265985088));
#13159=CARTESIAN_POINT('Ctrl Pts',(-0.548874290046456,-0.159766064500479,
0.813159949759));
#13160=CARTESIAN_POINT('Ctrl Pts',(-0.537715343527944,-0.142345102874864,
0.820511285096538));
#13161=CARTESIAN_POINT('Ctrl Pts',(-0.517157748491652,-0.0999305678883309,
0.833661031856294));
#13162=CARTESIAN_POINT('Ctrl Pts',(-0.508899795931835,-0.0740444353928835,
0.838633903678357));
#13163=CARTESIAN_POINT('Ctrl Pts',(-0.504455939115716,-0.04763,0.841298510752801));
#13164=CARTESIAN_POINT('Origin',(-0.707106781186548,-0.04763,0.707106781186547));
#13165=CARTESIAN_POINT('Origin',(0.,-0.04763,0.));
#13166=CARTESIAN_POINT('',(-0.951592097314,-0.04763,0.238183666596899));
#13167=CARTESIAN_POINT('Origin',(0.,-0.04763,0.));
#13168=CARTESIAN_POINT('Origin',(-1.,-0.04763,-1.11022302462516E-16));
#13169=CARTESIAN_POINT('Origin',(-1.,0.,-1.11022302462516E-16));
#13170=CARTESIAN_POINT('',(-0.951592097314,-0.04763,-0.2381836665969));
#13171=CARTESIAN_POINT('',(-0.980948,-0.246942143572133,1.08514323328844E-18));
#13172=CARTESIAN_POINT('Ctrl Pts',(-0.951592097314,-0.04763,-0.238183666596899));
#13173=CARTESIAN_POINT('Ctrl Pts',(-0.952850216871763,-0.0740444353928835,
-0.233157223576062));
#13174=CARTESIAN_POINT('Ctrl Pts',(-0.955173119738174,-0.0999305678883309,
-0.223801617934946));
#13175=CARTESIAN_POINT('Ctrl Pts',(-0.960411259488514,-0.142345102874864,
-0.199966927975188));
#13176=CARTESIAN_POINT('Ctrl Pts',(-0.963103647174702,-0.159766064500479,
-0.1868781821531));
#13177=CARTESIAN_POINT('Ctrl Pts',(-0.968453058988463,-0.190326085855194,
-0.15681442133453));
#13178=CARTESIAN_POINT('Ctrl Pts',(-0.971100730005489,-0.203463743702801,
-0.139836317888043));
#13179=CARTESIAN_POINT('Ctrl Pts',(-0.975530745318961,-0.224161999508995,
-0.104422493053067));
#13180=CARTESIAN_POINT('Ctrl Pts',(-0.977553872336861,-0.232861760990032,
-0.0842175114474175));
#13181=CARTESIAN_POINT('Ctrl Pts',(-0.980270995488453,-0.244251601209411,
-0.0421062857595699));
#13182=CARTESIAN_POINT('Ctrl Pts',(-0.980948,-0.246942143572133,-0.0201990724523195));
#13183=CARTESIAN_POINT('Ctrl Pts',(-0.980948,-0.246942143572133,-1.17961196366423E-16));
#13184=CARTESIAN_POINT('Origin',(-1.,-0.04763,-1.11022302462516E-16));
#13185=CARTESIAN_POINT('Ctrl Pts',(-0.980948,-0.246942143572133,-1.17961196366423E-16));
#13186=CARTESIAN_POINT('Ctrl Pts',(-0.980948,-0.246942143572133,0.0201990724523192));
#13187=CARTESIAN_POINT('Ctrl Pts',(-0.980270995488453,-0.244251601209411,
0.0421062857595695));
#13188=CARTESIAN_POINT('Ctrl Pts',(-0.977553872336861,-0.232861760990032,
0.0842175114474169));
#13189=CARTESIAN_POINT('Ctrl Pts',(-0.975530745318961,-0.224161999508995,
0.104422493053066));
#13190=CARTESIAN_POINT('Ctrl Pts',(-0.971100730005489,-0.203463743702801,
0.139836317888042));
#13191=CARTESIAN_POINT('Ctrl Pts',(-0.968453058988463,-0.190326085855194,
0.15681442133453));
#13192=CARTESIAN_POINT('Ctrl Pts',(-0.963103647174702,-0.15976606450048,
0.1868781821531));
#13193=CARTESIAN_POINT('Ctrl Pts',(-0.960411259488514,-0.142345102874864,
0.199966927975188));
#13194=CARTESIAN_POINT('Ctrl Pts',(-0.955173119738174,-0.099930567888331,
0.223801617934945));
#13195=CARTESIAN_POINT('Ctrl Pts',(-0.952850216871763,-0.0740444353928835,
0.233157223576061));
#13196=CARTESIAN_POINT('Ctrl Pts',(-0.951592097314,-0.04763,0.238183666596899));
#13197=CARTESIAN_POINT('Origin',(0.,-0.04763,0.));
#13198=CARTESIAN_POINT('',(-0.841298510752802,-0.04763,-0.504455939115715));
#13199=CARTESIAN_POINT('Origin',(0.,-0.04763,0.));
#13200=CARTESIAN_POINT('Origin',(-0.707106781186547,-0.04763,-0.707106781186548));
#13201=CARTESIAN_POINT('Origin',(-0.707106781186547,0.,-0.707106781186548));
#13202=CARTESIAN_POINT('',(-0.504455939115715,-0.04763,-0.841298510752802));
#13203=CARTESIAN_POINT('Ctrl Pts',(-0.504455939115715,-0.04763,-0.841298510752802));
#13204=CARTESIAN_POINT('Ctrl Pts',(-0.508899795931835,-0.0740444353928835,
-0.838633903678357));
#13205=CARTESIAN_POINT('Ctrl Pts',(-0.517157748491652,-0.0999305678883309,
-0.833661031856294));
#13206=CARTESIAN_POINT('Ctrl Pts',(-0.537715343527944,-0.142345102874864,
-0.820511285096538));
#13207=CARTESIAN_POINT('Ctrl Pts',(-0.548874290046456,-0.159766064500479,
-0.813159949759));
#13208=CARTESIAN_POINT('Ctrl Pts',(-0.573915184558107,-0.190326085855194,
-0.795684265985089));
#13209=CARTESIAN_POINT('Ctrl Pts',(-0.587792702767295,-0.203463743702801,
-0.78555112003688));
#13210=CARTESIAN_POINT('Ctrl Pts',(-0.615966552324775,-0.224161999508995,
-0.763642258217233));
#13211=CARTESIAN_POINT('Ctrl Pts',(-0.631684198665438,-0.232861760990032,
-0.750785745543687));
#13212=CARTESIAN_POINT('Ctrl Pts',(-0.663382628119203,-0.244251601209411,
-0.722929908501543));
#13213=CARTESIAN_POINT('Ctrl Pts',(-0.679352081686668,-0.246942143572133,
-0.707917883896095));
#13214=CARTESIAN_POINT('Ctrl Pts',(-0.707917883896095,-0.246942143572133,
-0.679352081686668));
#13215=CARTESIAN_POINT('Ctrl Pts',(-0.722929908501543,-0.244251601209411,
-0.663382628119203));
#13216=CARTESIAN_POINT('Ctrl Pts',(-0.750785745543687,-0.232861760990032,
-0.631684198665439));
#13217=CARTESIAN_POINT('Ctrl Pts',(-0.763642258217232,-0.224161999508995,
-0.615966552324775));
#13218=CARTESIAN_POINT('Ctrl Pts',(-0.78555112003688,-0.203463743702801,
-0.587792702767295));
#13219=CARTESIAN_POINT('Ctrl Pts',(-0.795684265985088,-0.190326085855194,
-0.573915184558107));
#13220=CARTESIAN_POINT('Ctrl Pts',(-0.813159949759,-0.15976606450048,-0.548874290046456));
#13221=CARTESIAN_POINT('Ctrl Pts',(-0.820511285096538,-0.142345102874864,
-0.537715343527944));
#13222=CARTESIAN_POINT('Ctrl Pts',(-0.833661031856294,-0.0999305678883311,
-0.517157748491652));
#13223=CARTESIAN_POINT('Ctrl Pts',(-0.838633903678357,-0.0740444353928836,
-0.508899795931835));
#13224=CARTESIAN_POINT('Ctrl Pts',(-0.841298510752801,-0.04763,-0.504455939115715));
#13225=CARTESIAN_POINT('Origin',(-0.707106781186547,-0.04763,-0.707106781186548));
#13226=CARTESIAN_POINT('Origin',(0.,-0.04763,0.));
#13227=CARTESIAN_POINT('',(-0.238183666596899,-0.04763,-0.951592097314));
#13228=CARTESIAN_POINT('Origin',(0.,-0.04763,0.));
#13229=CARTESIAN_POINT('Origin',(5.55111512312578E-17,-0.04763,-1.));
#13230=CARTESIAN_POINT('Origin',(5.55111512312578E-17,0.,-1.));
#13231=CARTESIAN_POINT('',(0.238183666596899,-0.04763,-0.951592097314));
#13232=CARTESIAN_POINT('Ctrl Pts',(0.238183666596899,-0.04763,-0.951592097314));
#13233=CARTESIAN_POINT('Ctrl Pts',(0.233157223576062,-0.0740444353928835,
-0.952850216871763));
#13234=CARTESIAN_POINT('Ctrl Pts',(0.223801617934946,-0.099930567888331,
-0.955173119738174));
#13235=CARTESIAN_POINT('Ctrl Pts',(0.199966927975188,-0.142345102874864,
-0.960411259488514));
#13236=CARTESIAN_POINT('Ctrl Pts',(0.1868781821531,-0.15976606450048,-0.963103647174702));
#13237=CARTESIAN_POINT('Ctrl Pts',(0.15681442133453,-0.190326085855194,
-0.968453058988463));
#13238=CARTESIAN_POINT('Ctrl Pts',(0.139836317888042,-0.203463743702801,
-0.971100730005489));
#13239=CARTESIAN_POINT('Ctrl Pts',(0.104422493053067,-0.224161999508995,
-0.975530745318961));
#13240=CARTESIAN_POINT('Ctrl Pts',(0.0842175114474173,-0.232861760990032,
-0.977553872336861));
#13241=CARTESIAN_POINT('Ctrl Pts',(0.0421062857595698,-0.244251601209411,
-0.980270995488453));
#13242=CARTESIAN_POINT('Ctrl Pts',(0.0201990724523194,-0.246942143572133,
-0.980948));
#13243=CARTESIAN_POINT('Ctrl Pts',(-0.0201990724523193,-0.246942143572133,
-0.980948));
#13244=CARTESIAN_POINT('Ctrl Pts',(-0.0421062857595697,-0.244251601209411,
-0.980270995488453));
#13245=CARTESIAN_POINT('Ctrl Pts',(-0.0842175114474171,-0.232861760990032,
-0.977553872336861));
#13246=CARTESIAN_POINT('Ctrl Pts',(-0.104422493053067,-0.224161999508995,
-0.975530745318961));
#13247=CARTESIAN_POINT('Ctrl Pts',(-0.139836317888042,-0.203463743702801,
-0.971100730005489));
#13248=CARTESIAN_POINT('Ctrl Pts',(-0.15681442133453,-0.190326085855194,
-0.968453058988463));
#13249=CARTESIAN_POINT('Ctrl Pts',(-0.1868781821531,-0.15976606450048,-0.963103647174702));
#13250=CARTESIAN_POINT('Ctrl Pts',(-0.199966927975188,-0.142345102874864,
-0.960411259488514));
#13251=CARTESIAN_POINT('Ctrl Pts',(-0.223801617934945,-0.099930567888331,
-0.955173119738174));
#13252=CARTESIAN_POINT('Ctrl Pts',(-0.233157223576062,-0.0740444353928835,
-0.952850216871763));
#13253=CARTESIAN_POINT('Ctrl Pts',(-0.238183666596899,-0.0476299999999999,
-0.951592097314));
#13254=CARTESIAN_POINT('Origin',(5.55111512312578E-17,-0.04763,-1.));
#13255=CARTESIAN_POINT('Origin',(0.,-0.04763,0.));
#13256=CARTESIAN_POINT('',(0.504455939115715,-0.04763,-0.841298510752802));
#13257=CARTESIAN_POINT('Origin',(0.,-0.04763,0.));
#13258=CARTESIAN_POINT('Origin',(0.707106781186548,-0.04763,-0.707106781186547));
#13259=CARTESIAN_POINT('Origin',(0.707106781186548,0.,-0.707106781186547));
#13260=CARTESIAN_POINT('',(0.841298510752802,-0.04763,-0.504455939115715));
#13261=CARTESIAN_POINT('Ctrl Pts',(0.841298510752802,-0.04763,-0.504455939115715));
#13262=CARTESIAN_POINT('Ctrl Pts',(0.838633903678357,-0.0740444353928835,
-0.508899795931835));
#13263=CARTESIAN_POINT('Ctrl Pts',(0.833661031856294,-0.0999305678883309,
-0.517157748491652));
#13264=CARTESIAN_POINT('Ctrl Pts',(0.820511285096538,-0.142345102874864,
-0.537715343527944));
#13265=CARTESIAN_POINT('Ctrl Pts',(0.813159949759,-0.159766064500479,-0.548874290046456));
#13266=CARTESIAN_POINT('Ctrl Pts',(0.795684265985088,-0.190326085855194,
-0.573915184558107));
#13267=CARTESIAN_POINT('Ctrl Pts',(0.78555112003688,-0.203463743702801,
-0.587792702767295));
#13268=CARTESIAN_POINT('Ctrl Pts',(0.763642258217233,-0.224161999508995,
-0.615966552324775));
#13269=CARTESIAN_POINT('Ctrl Pts',(0.750785745543687,-0.232861760990032,
-0.631684198665438));
#13270=CARTESIAN_POINT('Ctrl Pts',(0.722929908501543,-0.244251601209411,
-0.663382628119203));
#13271=CARTESIAN_POINT('Ctrl Pts',(0.707917883896095,-0.246942143572133,
-0.679352081686668));
#13272=CARTESIAN_POINT('Ctrl Pts',(0.679352081686668,-0.246942143572133,
-0.707917883896095));
#13273=CARTESIAN_POINT('Ctrl Pts',(0.663382628119203,-0.244251601209411,
-0.722929908501543));
#13274=CARTESIAN_POINT('Ctrl Pts',(0.631684198665438,-0.232861760990032,
-0.750785745543687));
#13275=CARTESIAN_POINT('Ctrl Pts',(0.615966552324775,-0.224161999508995,
-0.763642258217232));
#13276=CARTESIAN_POINT('Ctrl Pts',(0.587792702767295,-0.203463743702801,
-0.78555112003688));
#13277=CARTESIAN_POINT('Ctrl Pts',(0.573915184558107,-0.190326085855194,
-0.795684265985088));
#13278=CARTESIAN_POINT('Ctrl Pts',(0.548874290046456,-0.159766064500479,
-0.813159949759));
#13279=CARTESIAN_POINT('Ctrl Pts',(0.537715343527944,-0.142345102874864,
-0.820511285096538));
#13280=CARTESIAN_POINT('Ctrl Pts',(0.517157748491652,-0.099930567888331,
-0.833661031856294));
#13281=CARTESIAN_POINT('Ctrl Pts',(0.508899795931835,-0.0740444353928835,
-0.838633903678357));
#13282=CARTESIAN_POINT('Ctrl Pts',(0.504455939115715,-0.04763,-0.841298510752801));
#13283=CARTESIAN_POINT('Origin',(0.707106781186548,-0.04763,-0.707106781186547));
#13284=CARTESIAN_POINT('Origin',(0.,-0.166705,0.));
#13285=CARTESIAN_POINT('',(-0.980948,-0.28578,1.20131482833E-16));
#13286=CARTESIAN_POINT('Origin',(0.,-0.28578,0.));
#13287=CARTESIAN_POINT('',(-0.980948,-0.166705,1.20131482833E-16));
#13288=CARTESIAN_POINT('',(0.951592097314,-0.04763,0.238183666596899));
#13289=CARTESIAN_POINT('Origin',(0.,-0.04763,0.));
#13290=CARTESIAN_POINT('',(0.951592097314,-0.04763,-0.238183666596899));
#13291=CARTESIAN_POINT('Ctrl Pts',(0.951592097314,-0.04763,0.238183666596899));
#13292=CARTESIAN_POINT('Ctrl Pts',(0.952850216871763,-0.0740444353928835,
0.233157223576062));
#13293=CARTESIAN_POINT('Ctrl Pts',(0.955173119738174,-0.099930567888331,
0.223801617934945));
#13294=CARTESIAN_POINT('Ctrl Pts',(0.960411259488514,-0.142345102874864,
0.199966927975188));
#13295=CARTESIAN_POINT('Ctrl Pts',(0.963103647174702,-0.15976606450048,
0.1868781821531));
#13296=CARTESIAN_POINT('Ctrl Pts',(0.968453058988463,-0.190326085855194,
0.15681442133453));
#13297=CARTESIAN_POINT('Ctrl Pts',(0.971100730005489,-0.203463743702801,
0.139836317888042));
#13298=CARTESIAN_POINT('Ctrl Pts',(0.975530745318961,-0.224161999508995,
0.104422493053067));
#13299=CARTESIAN_POINT('Ctrl Pts',(0.977553872336861,-0.232861760990032,
0.0842175114474172));
#13300=CARTESIAN_POINT('Ctrl Pts',(0.980270995488453,-0.244251601209411,
0.0421062857595697));
#13301=CARTESIAN_POINT('Ctrl Pts',(0.980948,-0.246942143572133,0.0201990724523194));
#13302=CARTESIAN_POINT('Ctrl Pts',(0.980948,-0.246942143572133,-0.0201990724523194));
#13303=CARTESIAN_POINT('Ctrl Pts',(0.980270995488453,-0.244251601209411,
-0.0421062857595697));
#13304=CARTESIAN_POINT('Ctrl Pts',(0.977553872336861,-0.232861760990032,
-0.0842175114474172));
#13305=CARTESIAN_POINT('Ctrl Pts',(0.975530745318961,-0.224161999508995,
-0.104422493053067));
#13306=CARTESIAN_POINT('Ctrl Pts',(0.971100730005489,-0.203463743702801,
-0.139836317888042));
#13307=CARTESIAN_POINT('Ctrl Pts',(0.968453058988463,-0.190326085855194,
-0.15681442133453));
#13308=CARTESIAN_POINT('Ctrl Pts',(0.963103647174702,-0.15976606450048,
-0.1868781821531));
#13309=CARTESIAN_POINT('Ctrl Pts',(0.960411259488514,-0.142345102874864,
-0.199966927975188));
#13310=CARTESIAN_POINT('Ctrl Pts',(0.955173119738174,-0.099930567888331,
-0.223801617934945));
#13311=CARTESIAN_POINT('Ctrl Pts',(0.952850216871763,-0.0740444353928835,
-0.233157223576062));
#13312=CARTESIAN_POINT('Ctrl Pts',(0.951592097314,-0.0476299999999999,-0.238183666596899));
#13313=CARTESIAN_POINT('Origin',(0.,-0.04763,0.));
#13314=CARTESIAN_POINT('Origin',(0.,-0.04763,0.));
#13315=CARTESIAN_POINT('Origin',(1.,-0.04763,0.));
#13316=CARTESIAN_POINT('Origin',(1.,0.,0.));
#13317=CARTESIAN_POINT('Origin',(1.,-0.04763,0.));
#13318=CARTESIAN_POINT('Origin',(0.,-0.28578,0.));
#13319=CARTESIAN_POINT('Origin',(0.,-0.04763,0.));
#13320=CARTESIAN_POINT('',(0.,0.,0.));
#13321=CARTESIAN_POINT('Origin',(1.013815,0.445,0.));
#13322=CARTESIAN_POINT('',(-1.013815,0.445,-1.24156529467757E-16));
#13323=CARTESIAN_POINT('Origin',(0.,0.445,0.));
#13324=CARTESIAN_POINT('',(-0.991185,0.445,-1.21385153761287E-16));
#13325=CARTESIAN_POINT('Origin',(0.,0.445,0.));
#13326=CARTESIAN_POINT('Origin',(0.,0.4075,0.));
#13327=CARTESIAN_POINT('',(-1.013815,0.37,-1.24156529467757E-16));
#13328=CARTESIAN_POINT('Origin',(0.,0.37,0.));
#13329=CARTESIAN_POINT('',(-1.013815,0.4075,-1.24156529467757E-16));
#13330=CARTESIAN_POINT('Origin',(0.991185,0.37,0.));
#13331=CARTESIAN_POINT('',(-0.991185,0.37,-1.21385153761287E-16));
#13332=CARTESIAN_POINT('Origin',(0.,0.37,0.));
#13333=CARTESIAN_POINT('Origin',(0.,0.4075,0.));
#13334=CARTESIAN_POINT('',(-0.991185,0.4075,-1.21385153761287E-16));
#13335=CARTESIAN_POINT('Origin',(1.013815,-0.37,0.));
#13336=CARTESIAN_POINT('',(-1.013815,-0.37,-1.24156529467757E-16));
#13337=CARTESIAN_POINT('Origin',(0.,-0.37,0.));
#13338=CARTESIAN_POINT('',(-0.991185,-0.37,-1.21385153761287E-16));
#13339=CARTESIAN_POINT('Origin',(0.,-0.37,0.));
#13340=CARTESIAN_POINT('Origin',(0.,-0.4075,0.));
#13341=CARTESIAN_POINT('',(-1.013815,-0.445,-1.24156529467757E-16));
#13342=CARTESIAN_POINT('Origin',(0.,-0.445,0.));
#13343=CARTESIAN_POINT('',(-1.013815,-0.4075,-1.24156529467757E-16));
#13344=CARTESIAN_POINT('Origin',(0.991185,-0.445,0.));
#13345=CARTESIAN_POINT('',(-0.991185,-0.445,-1.21385153761287E-16));
#13346=CARTESIAN_POINT('Origin',(0.,-0.445,0.));
#13347=CARTESIAN_POINT('Origin',(0.,-0.4075,0.));
#13348=CARTESIAN_POINT('',(-0.991185,-0.4075,-1.21385153761287E-16));
#13349=CARTESIAN_POINT('',(0.,0.,0.));
#13350=CARTESIAN_POINT('',(0.,0.,0.));
#13351=CARTESIAN_POINT('',(0.,0.,0.));
#13352=CARTESIAN_POINT('',(0.,0.,0.));
#13353=CARTESIAN_POINT('',(0.,0.,0.));
#13354=CARTESIAN_POINT('',(0.,0.,0.));
#13355=CARTESIAN_POINT('Origin',(3.,29.95,8.));
#13356=CARTESIAN_POINT('',(2.495,31.,8.));
#13357=CARTESIAN_POINT('Origin',(3.,31.,8.));
#13358=CARTESIAN_POINT('',(2.495,29.95,8.));
#13359=CARTESIAN_POINT('',(2.495,29.95,8.));
#13360=CARTESIAN_POINT('Origin',(3.,29.95,8.));
#13361=CARTESIAN_POINT('Origin',(3.,29.95,8.));
#13362=CARTESIAN_POINT('',(2.3,31.,8.));
#13363=CARTESIAN_POINT('Origin',(3.,31.,8.));
#13364=CARTESIAN_POINT('',(2.3,29.95,8.));
#13365=CARTESIAN_POINT('',(2.3,29.95,8.));
#13366=CARTESIAN_POINT('Origin',(3.,29.95,8.));
#13367=CARTESIAN_POINT('Origin',(3.,31.,8.));
#13368=CARTESIAN_POINT('Origin',(3.,29.95,8.));
#13369=CARTESIAN_POINT('',(0.,0.,0.));
#13370=CARTESIAN_POINT('Origin',(0.0866025403784439,-0.4,-0.15));
#13371=CARTESIAN_POINT('',(0.173205080756888,-0.4,0.));
#13372=CARTESIAN_POINT('',(0.0866025403784439,-0.4,-0.15));
#13373=CARTESIAN_POINT('',(0.173205080756888,-0.4,0.));
#13374=CARTESIAN_POINT('',(0.0866025403784439,-0.64,-0.15));
#13375=CARTESIAN_POINT('',(0.0866025403784439,-0.4,-0.15));
#13376=CARTESIAN_POINT('',(0.173205080756888,-0.64,0.));
#13377=CARTESIAN_POINT('',(0.173205080756888,-0.64,0.));
#13378=CARTESIAN_POINT('',(0.173205080756888,-0.4,0.));
#13379=CARTESIAN_POINT('Origin',(-0.0866025403784438,-0.4,-0.15));
#13380=CARTESIAN_POINT('',(-0.0866025403784438,-0.4,-0.15));
#13381=CARTESIAN_POINT('',(0.0866025403784439,-0.4,-0.15));
#13382=CARTESIAN_POINT('',(-0.0866025403784438,-0.64,-0.15));
#13383=CARTESIAN_POINT('',(-0.0866025403784438,-0.4,-0.15));
#13384=CARTESIAN_POINT('',(0.0866025403784439,-0.64,-0.15));
#13385=CARTESIAN_POINT('Origin',(-0.173205080756888,-0.4,-2.77555756156289E-17));
#13386=CARTESIAN_POINT('',(-0.173205080756888,-0.4,-2.12115047744981E-17));
#13387=CARTESIAN_POINT('',(-0.0866025403784438,-0.4,-0.15));
#13388=CARTESIAN_POINT('',(-0.173205080756888,-0.64,-2.77555756156289E-17));
#13389=CARTESIAN_POINT('',(-0.173205080756888,-0.4,-2.12115047744981E-17));
#13390=CARTESIAN_POINT('',(-0.0866025403784438,-0.64,-0.15));
#13391=CARTESIAN_POINT('Origin',(-0.0866025403784439,-0.4,0.15));
#13392=CARTESIAN_POINT('',(-0.0866025403784439,-0.4,0.15));
#13393=CARTESIAN_POINT('',(-0.173205080756888,-0.4,-2.12115047744981E-17));
#13394=CARTESIAN_POINT('',(-0.0866025403784439,-0.64,0.15));
#13395=CARTESIAN_POINT('',(-0.0866025403784439,-0.4,0.15));
#13396=CARTESIAN_POINT('',(-0.173205080756888,-0.64,-2.12115047744981E-17));
#13397=CARTESIAN_POINT('Origin',(0.0866025403784439,-0.4,0.15));
#13398=CARTESIAN_POINT('',(0.0866025403784439,-0.4,0.15));
#13399=CARTESIAN_POINT('',(-0.0866025403784439,-0.4,0.15));
#13400=CARTESIAN_POINT('',(0.0866025403784439,-0.64,0.15));
#13401=CARTESIAN_POINT('',(0.0866025403784439,-0.4,0.15));
#13402=CARTESIAN_POINT('',(-0.0866025403784439,-0.64,0.15));
#13403=CARTESIAN_POINT('Origin',(0.173205080756888,-0.4,0.));
#13404=CARTESIAN_POINT('',(0.0866025403784439,-0.4,0.15));
#13405=CARTESIAN_POINT('',(0.0866025403784439,-0.64,0.15));
#13406=CARTESIAN_POINT('Origin',(0.,-0.4,-2.77555756156289E-17));
#13407=CARTESIAN_POINT('Origin',(0.,-0.64,-2.77555756156289E-17));
#13408=CARTESIAN_POINT('Origin',(0.,-1.,0.));
#13409=CARTESIAN_POINT('',(-0.1954,-1.,2.39295984553393E-17));
#13410=CARTESIAN_POINT('Origin',(0.,-1.,0.));
#13411=CARTESIAN_POINT('Origin',(0.3,0.4,0.));
#13412=CARTESIAN_POINT('',(-0.3,0.4,-3.67394039744206E-17));
#13413=CARTESIAN_POINT('Origin',(0.,0.4,0.));
#13414=CARTESIAN_POINT('Origin',(0.,0.375,0.));
#13415=CARTESIAN_POINT('',(-0.35,0.35,-4.28626379701573E-17));
#13416=CARTESIAN_POINT('Origin',(0.,0.35,0.));
#13417=CARTESIAN_POINT('',(-0.325,0.375,-3.9801020972289E-17));
#13418=CARTESIAN_POINT('Origin',(0.,0.19,0.));
#13419=CARTESIAN_POINT('',(-0.35,0.03,-4.28626379701574E-17));
#13420=CARTESIAN_POINT('Origin',(0.,0.03,0.));
#13421=CARTESIAN_POINT('',(-0.35,0.19,-4.28626379701574E-17));
#13422=CARTESIAN_POINT('Origin',(0.,0.0149999999999999,0.));
#13423=CARTESIAN_POINT('',(-0.32,-3.29597460435593E-17,-3.91886975727153E-17));
#13424=CARTESIAN_POINT('Origin',(0.,0.,0.));
#13425=CARTESIAN_POINT('',(-0.335,0.0149999999999999,-4.10256677714363E-17));
#13426=CARTESIAN_POINT('Origin',(0.22,0.,0.));
#13427=CARTESIAN_POINT('',(-0.22,-6.93889390390723E-18,-2.69422295812418E-17));
#13428=CARTESIAN_POINT('Origin',(0.,0.,0.));
#13429=CARTESIAN_POINT('Origin',(0.,-0.02,0.));
#13430=CARTESIAN_POINT('',(-0.1954,-0.0492,2.39295984553393E-17));
#13431=CARTESIAN_POINT('Origin',(0.,-0.0492,0.));
#13432=CARTESIAN_POINT('',(-0.21,-0.02,-2.57175827820944E-17));
#13433=CARTESIAN_POINT('Origin',(0.,-0.8,0.));
#13434=CARTESIAN_POINT('',(-0.1954,-0.8,-2.39295984553393E-17));
#13435=CARTESIAN_POINT('',(0.,0.,0.));
#13436=CARTESIAN_POINT('Origin',(3.,33.,8.));
#13437=CARTESIAN_POINT('',(2.775,33.2,8.));
#13438=CARTESIAN_POINT('Origin',(3.,33.2,8.));
#13439=CARTESIAN_POINT('',(2.775,33.,8.));
#13440=CARTESIAN_POINT('',(2.775,33.,8.));
#13441=CARTESIAN_POINT('Origin',(3.,33.,8.));
#13442=CARTESIAN_POINT('Origin',(3.,33.,8.));
#13443=CARTESIAN_POINT('',(2.3,33.2,8.));
#13444=CARTESIAN_POINT('Origin',(3.,33.2,8.));
#13445=CARTESIAN_POINT('',(2.3,33.,8.));
#13446=CARTESIAN_POINT('',(2.3,33.,8.));
#13447=CARTESIAN_POINT('Origin',(3.,33.,8.));
#13448=CARTESIAN_POINT('Origin',(3.,33.2,8.));
#13449=CARTESIAN_POINT('Origin',(3.,33.,8.));
#13450=CARTESIAN_POINT('',(0.,0.,0.));
#13451=CARTESIAN_POINT('Origin',(0.,0.395,0.25));
#13452=CARTESIAN_POINT('',(-0.5,0.3,0.25));
#13453=CARTESIAN_POINT('',(0.5,0.3,0.25));
#13454=CARTESIAN_POINT('',(0.25,0.3,0.25));
#13455=CARTESIAN_POINT('',(-0.5,0.5,0.25));
#13456=CARTESIAN_POINT('',(-0.5,0.5,0.25));
#13457=CARTESIAN_POINT('',(0.5,0.5,0.25));
#13458=CARTESIAN_POINT('',(0.5,0.5,0.25));
#13459=CARTESIAN_POINT('',(0.5,0.29,0.25));
#13460=CARTESIAN_POINT('Origin',(0.5,0.5,0.25));
#13461=CARTESIAN_POINT('',(-0.5,0.5,0.4));
#13462=CARTESIAN_POINT('',(-0.5,0.5,0.25));
#13463=CARTESIAN_POINT('',(0.5,0.5,0.4));
#13464=CARTESIAN_POINT('',(0.5,0.5,0.4));
#13465=CARTESIAN_POINT('',(0.5,0.5,0.25));
#13466=CARTESIAN_POINT('Origin',(0.,0.,0.4));
#13467=CARTESIAN_POINT('',(-0.5,-0.5,0.4));
#13468=CARTESIAN_POINT('',(-0.5,0.5,0.4));
#13469=CARTESIAN_POINT('',(0.5,-0.5,0.4));
#13470=CARTESIAN_POINT('',(-0.5,-0.5,0.4));
#13471=CARTESIAN_POINT('',(0.5,-0.3,0.4));
#13472=CARTESIAN_POINT('',(-0.2117,2.59257727379495E-17,0.4));
#13473=CARTESIAN_POINT('Origin',(0.,0.,0.4));
#13474=CARTESIAN_POINT('Origin',(-0.5,0.3,0.));
#13475=CARTESIAN_POINT('',(-0.5,0.3,0.15));
#13476=CARTESIAN_POINT('',(-0.5,0.3,0.));
#13477=CARTESIAN_POINT('',(-0.5,0.15,0.));
#13478=CARTESIAN_POINT('',(-0.5,0.225,0.075));
#13479=CARTESIAN_POINT('',(-0.5,-0.15,0.));
#13480=CARTESIAN_POINT('',(-0.5,0.3,0.));
#13481=CARTESIAN_POINT('',(-0.5,-0.3,0.15));
#13482=CARTESIAN_POINT('',(-0.5,-0.075,-0.075));
#13483=CARTESIAN_POINT('',(-0.5,-0.3,0.25));
#13484=CARTESIAN_POINT('',(-0.5,-0.3,0.));
#13485=CARTESIAN_POINT('',(-0.5,-0.5,0.25));
#13486=CARTESIAN_POINT('',(-0.5,-0.29,0.25));
#13487=CARTESIAN_POINT('',(-0.5,-0.5,0.25));
#13488=CARTESIAN_POINT('Origin',(-0.5,-0.5,0.25));
#13489=CARTESIAN_POINT('',(0.5,-0.5,0.25));
#13490=CARTESIAN_POINT('',(-0.5,-0.5,0.25));
#13491=CARTESIAN_POINT('',(0.5,-0.5,0.25));
#13492=CARTESIAN_POINT('Origin',(0.,-0.395,0.25));
#13493=CARTESIAN_POINT('',(0.5,-0.3,0.25));
#13494=CARTESIAN_POINT('',(-0.25,-0.3,0.25));
#13495=CARTESIAN_POINT('',(0.5,-0.5,0.25));
#13496=CARTESIAN_POINT('Origin',(0.5,-0.3,0.));
#13497=CARTESIAN_POINT('',(0.5,-0.3,0.15));
#13498=CARTESIAN_POINT('',(0.5,-0.3,0.));
#13499=CARTESIAN_POINT('',(0.5,-0.15,0.));
#13500=CARTESIAN_POINT('',(0.5,-0.225,0.075));
#13501=CARTESIAN_POINT('',(0.5,0.15,0.));
#13502=CARTESIAN_POINT('',(0.5,-0.3,0.));
#13503=CARTESIAN_POINT('',(0.5,0.3,0.15));
#13504=CARTESIAN_POINT('',(0.5,0.075,-0.075));
#13505=CARTESIAN_POINT('',(0.5,0.3,0.));
#13506=CARTESIAN_POINT('Origin',(-0.5,-0.3,0.));
#13507=CARTESIAN_POINT('',(-0.25,-0.3,0.15));
#13508=CARTESIAN_POINT('Origin',(-0.25,-0.225,0.075));
#13509=CARTESIAN_POINT('',(-0.149388386429468,-0.15,0.));
#13510=CARTESIAN_POINT('',(-0.25,-0.15,0.));
#13511=CARTESIAN_POINT('',(0.149388386429468,-0.15,0.));
#13512=CARTESIAN_POINT('Origin',(0.,0.,-0.15));
#13513=CARTESIAN_POINT('',(-0.25,-0.15,0.));
#13514=CARTESIAN_POINT('Origin',(0.,0.,-0.1));
#13515=CARTESIAN_POINT('',(-0.2117,-2.59257727379495E-17,0.));
#13516=CARTESIAN_POINT('Origin',(0.,0.,0.));
#13517=CARTESIAN_POINT('',(-0.2117,-2.59257727379495E-17,-0.1));
#13518=CARTESIAN_POINT('',(-0.149388386429468,0.15,0.));
#13519=CARTESIAN_POINT('Origin',(0.,0.,0.));
#13520=CARTESIAN_POINT('',(0.149388386429468,0.15,0.));
#13521=CARTESIAN_POINT('Origin',(0.,0.,-0.15));
#13522=CARTESIAN_POINT('Origin',(0.,0.,0.));
#13523=CARTESIAN_POINT('Origin',(0.,0.,0.));
#13524=CARTESIAN_POINT('',(0.25,0.15,0.));
#13525=CARTESIAN_POINT('Origin',(0.,0.,0.));
#13526=CARTESIAN_POINT('',(0.25,0.15,0.));
#13527=CARTESIAN_POINT('Origin',(0.25,0.225,0.075));
#13528=CARTESIAN_POINT('',(0.25,0.3,0.15));
#13529=CARTESIAN_POINT('Origin',(0.5,0.3,0.));
#13530=CARTESIAN_POINT('',(0.,0.,0.));
#13531=CARTESIAN_POINT('Origin',(0.115470053837925,-0.5,-0.2));
#13532=CARTESIAN_POINT('',(0.23094010767585,-0.5,0.));
#13533=CARTESIAN_POINT('',(0.115470053837925,-0.5,-0.2));
#13534=CARTESIAN_POINT('',(0.23094010767585,-0.5,0.));
#13535=CARTESIAN_POINT('',(0.115470053837925,-0.8,-0.2));
#13536=CARTESIAN_POINT('',(0.115470053837925,-0.5,-0.2));
#13537=CARTESIAN_POINT('',(0.23094010767585,-0.8,0.));
#13538=CARTESIAN_POINT('',(0.23094010767585,-0.8,0.));
#13539=CARTESIAN_POINT('',(0.23094010767585,-0.5,0.));
#13540=CARTESIAN_POINT('Origin',(-0.115470053837925,-0.5,-0.2));
#13541=CARTESIAN_POINT('',(-0.115470053837925,-0.5,-0.2));
#13542=CARTESIAN_POINT('',(0.115470053837925,-0.5,-0.2));
#13543=CARTESIAN_POINT('',(-0.115470053837925,-0.8,-0.2));
#13544=CARTESIAN_POINT('',(-0.115470053837925,-0.5,-0.2));
#13545=CARTESIAN_POINT('',(0.115470053837925,-0.8,-0.2));
#13546=CARTESIAN_POINT('Origin',(-0.23094010767585,-0.5,-2.77555756156289E-17));
#13547=CARTESIAN_POINT('',(-0.23094010767585,-0.5,-2.82820063659975E-17));
#13548=CARTESIAN_POINT('',(-0.115470053837925,-0.5,-0.2));
#13549=CARTESIAN_POINT('',(-0.23094010767585,-0.8,-2.77555756156289E-17));
#13550=CARTESIAN_POINT('',(-0.23094010767585,-0.5,-2.82820063659975E-17));
#13551=CARTESIAN_POINT('',(-0.115470053837925,-0.8,-0.2));
#13552=CARTESIAN_POINT('Origin',(-0.115470053837925,-0.5,0.2));
#13553=CARTESIAN_POINT('',(-0.115470053837925,-0.5,0.2));
#13554=CARTESIAN_POINT('',(-0.23094010767585,-0.5,-2.82820063659975E-17));
#13555=CARTESIAN_POINT('',(-0.115470053837925,-0.8,0.2));
#13556=CARTESIAN_POINT('',(-0.115470053837925,-0.5,0.2));
#13557=CARTESIAN_POINT('',(-0.23094010767585,-0.8,-2.82820063659975E-17));
#13558=CARTESIAN_POINT('Origin',(0.115470053837925,-0.5,0.2));
#13559=CARTESIAN_POINT('',(0.115470053837925,-0.5,0.2));
#13560=CARTESIAN_POINT('',(-0.115470053837925,-0.5,0.2));
#13561=CARTESIAN_POINT('',(0.115470053837925,-0.8,0.2));
#13562=CARTESIAN_POINT('',(0.115470053837925,-0.5,0.2));
#13563=CARTESIAN_POINT('',(-0.115470053837925,-0.8,0.2));
#13564=CARTESIAN_POINT('Origin',(0.23094010767585,-0.5,0.));
#13565=CARTESIAN_POINT('',(0.115470053837925,-0.5,0.2));
#13566=CARTESIAN_POINT('',(0.115470053837925,-0.8,0.2));
#13567=CARTESIAN_POINT('Origin',(0.,-0.5,0.));
#13568=CARTESIAN_POINT('Origin',(0.,-0.8,0.));
#13569=CARTESIAN_POINT('Origin',(0.,-1.4,0.));
#13570=CARTESIAN_POINT('',(-0.24505,-1.4,3.00099698131059E-17));
#13571=CARTESIAN_POINT('Origin',(0.,-1.4,0.));
#13572=CARTESIAN_POINT('Origin',(0.375,0.5,0.));
#13573=CARTESIAN_POINT('',(-0.375,0.5,-4.59242549680257E-17));
#13574=CARTESIAN_POINT('Origin',(0.,0.5,0.));
#13575=CARTESIAN_POINT('Origin',(0.,0.475,0.));
#13576=CARTESIAN_POINT('',(-0.425,0.45,-5.20474889637625E-17));
#13577=CARTESIAN_POINT('Origin',(0.,0.45,0.));
#13578=CARTESIAN_POINT('',(-0.4,0.475,-4.89858719658941E-17));
#13579=CARTESIAN_POINT('Origin',(0.,0.24,0.));
#13580=CARTESIAN_POINT('',(-0.425,0.0299999999999998,-5.20474889637625E-17));
#13581=CARTESIAN_POINT('Origin',(0.,0.0299999999999998,0.));
#13582=CARTESIAN_POINT('',(-0.425,0.24,-5.20474889637625E-17));
#13583=CARTESIAN_POINT('Origin',(0.,0.0150000000000001,0.));
#13584=CARTESIAN_POINT('',(-0.395,4.85722573273506E-17,-4.83735485663204E-17));
#13585=CARTESIAN_POINT('Origin',(0.,0.,0.));
#13586=CARTESIAN_POINT('',(-0.41,0.0150000000000001,-5.02105187650415E-17));
#13587=CARTESIAN_POINT('Origin',(0.27,0.,0.));
#13588=CARTESIAN_POINT('',(-0.27,0.,-3.30654635769785E-17));
#13589=CARTESIAN_POINT('Origin',(0.,0.,0.));
#13590=CARTESIAN_POINT('Origin',(0.,-0.02,0.));
#13591=CARTESIAN_POINT('',(-0.24505,-0.0498999999999999,3.00099698131059E-17));
#13592=CARTESIAN_POINT('Origin',(0.,-0.0498999999999999,0.));
#13593=CARTESIAN_POINT('',(-0.26,-0.02,-3.18408167778312E-17));
#13594=CARTESIAN_POINT('Origin',(0.,-0.995,0.));
#13595=CARTESIAN_POINT('',(-0.24505,-0.995,-3.00099698131059E-17));
#13596=CARTESIAN_POINT('',(0.,-2.,5.));
#13597=CARTESIAN_POINT('',(40.,-2.,5.));
#13598=CARTESIAN_POINT('',(6.,-2.,-16.));
#13599=CARTESIAN_POINT('',(6.,-2.,6.));
#13600=CARTESIAN_POINT('',(6.,-2.,6.1));
#13601=CARTESIAN_POINT('',(6.,-2.,-16.8));
#13602=CARTESIAN_POINT('',(6.,-2.,-16.9));
#13603=CARTESIAN_POINT('',(54.,-2.,-16.));
#13604=CARTESIAN_POINT('',(54.,-2.,6.));
#13605=CARTESIAN_POINT('',(54.,-2.,6.1));
#13606=CARTESIAN_POINT('',(54.,-2.,-16.8));
#13607=CARTESIAN_POINT('',(54.,-2.,-16.9));
#13608=CARTESIAN_POINT('',(0.,0.,0.));
#13609=CARTESIAN_POINT('',(36.,-2.42,5.));
#13610=CARTESIAN_POINT('',(36.,-3.8,5.));
#13611=CARTESIAN_POINT('',(36.,-3.9,5.));
#13612=CARTESIAN_POINT('',(39.,-2.42,5.));
#13613=CARTESIAN_POINT('',(39.,-3.8,5.));
#13614=CARTESIAN_POINT('',(39.,-3.9,5.));
#13615=CARTESIAN_POINT('',(42.,-2.42,5.));
#13616=CARTESIAN_POINT('',(42.,-3.8,5.));
#13617=CARTESIAN_POINT('',(42.,-3.9,5.));
#13618=CARTESIAN_POINT('',(45.,-2.42,5.));
#13619=CARTESIAN_POINT('',(45.,-3.8,5.));
#13620=CARTESIAN_POINT('',(45.,-3.9,5.));
#13621=CARTESIAN_POINT('',(0.,32.,5.));
#13622=CARTESIAN_POINT('',(40.,32.,5.));
#13623=CARTESIAN_POINT('',(6.,32.,-16.));
#13624=CARTESIAN_POINT('',(6.,32.,6.));
#13625=CARTESIAN_POINT('',(6.,32.,6.1));
#13626=CARTESIAN_POINT('',(6.,32.,-16.8));
#13627=CARTESIAN_POINT('',(6.,32.,-16.9));
#13628=CARTESIAN_POINT('',(54.,32.,-16.));
#13629=CARTESIAN_POINT('',(54.,32.,6.));
#13630=CARTESIAN_POINT('',(54.,32.,6.1));
#13631=CARTESIAN_POINT('',(54.,32.,-16.8));
#13632=CARTESIAN_POINT('',(54.,32.,-16.9));
#13633=CARTESIAN_POINT('',(0.,0.,0.));
#13634=CARTESIAN_POINT('',(36.,32.42,5.));
#13635=CARTESIAN_POINT('',(36.,33.8,5.));
#13636=CARTESIAN_POINT('',(36.,33.9,5.));
#13637=CARTESIAN_POINT('',(39.,32.42,5.));
#13638=CARTESIAN_POINT('',(39.,33.8,5.));
#13639=CARTESIAN_POINT('',(39.,33.9,5.));
#13640=CARTESIAN_POINT('',(42.,32.42,5.));
#13641=CARTESIAN_POINT('',(42.,33.8,5.));
#13642=CARTESIAN_POINT('',(42.,33.9,5.));
#13643=CARTESIAN_POINT('',(45.,32.42,5.));
#13644=CARTESIAN_POINT('',(45.,33.8,5.));
#13645=CARTESIAN_POINT('',(45.,33.9,5.));
#13646=CARTESIAN_POINT('',(0.,0.,0.));
#13647=CARTESIAN_POINT('',(0.,0.,0.));
#13648=CARTESIAN_POINT('',(0.,0.,0.));
#13649=CARTESIAN_POINT('',(0.,0.,0.));
#13650=CARTESIAN_POINT('',(0.,0.,0.));
#13651=CARTESIAN_POINT('',(0.,0.,0.));
#13652=CARTESIAN_POINT('',(0.,0.,0.));
#13653=CARTESIAN_POINT('Origin',(1.6,32.,6.9));
#13654=CARTESIAN_POINT('',(1.1,32.,6.9));
#13655=CARTESIAN_POINT('Origin',(1.6,32.,6.9));
#13656=CARTESIAN_POINT('',(1.1,32.,9.));
#13657=CARTESIAN_POINT('',(1.1,32.,6.9));
#13658=CARTESIAN_POINT('Origin',(1.6,32.,9.));
#13659=CARTESIAN_POINT('Origin',(1.6,32.,6.9));
#13660=CARTESIAN_POINT('',(1.325,32.,6.9));
#13661=CARTESIAN_POINT('Origin',(1.6,32.,6.9));
#13662=CARTESIAN_POINT('Origin',(4.4,32.,6.9));
#13663=CARTESIAN_POINT('',(3.9,32.,6.9));
#13664=CARTESIAN_POINT('Origin',(4.4,32.,6.9));
#13665=CARTESIAN_POINT('',(3.9,32.,9.));
#13666=CARTESIAN_POINT('',(3.9,32.,6.9));
#13667=CARTESIAN_POINT('Origin',(4.4,32.,9.));
#13668=CARTESIAN_POINT('Origin',(4.4,32.,6.9));
#13669=CARTESIAN_POINT('',(4.125,32.,6.9));
#13670=CARTESIAN_POINT('Origin',(4.4,32.,6.9));
#13671=CARTESIAN_POINT('Origin',(1.6,32.,5.9));
#13672=CARTESIAN_POINT('',(1.325,32.,6.));
#13673=CARTESIAN_POINT('Origin',(1.6,32.,6.));
#13674=CARTESIAN_POINT('',(1.325,32.,5.9));
#13675=CARTESIAN_POINT('Origin',(4.4,32.,5.9));
#13676=CARTESIAN_POINT('',(4.125,32.,6.));
#13677=CARTESIAN_POINT('Origin',(4.4,32.,6.));
#13678=CARTESIAN_POINT('',(4.125,32.,5.9));
#13679=CARTESIAN_POINT('Origin',(3.,30.9,8.));
#13680=CARTESIAN_POINT('',(2.495,31.,8.));
#13681=CARTESIAN_POINT('Origin',(3.,31.,8.));
#13682=CARTESIAN_POINT('',(2.495,33.,8.));
#13683=CARTESIAN_POINT('',(2.495,30.9,8.));
#13684=CARTESIAN_POINT('Origin',(3.,33.,8.));
#13685=CARTESIAN_POINT('Origin',(5.,33.,6.));
#13686=CARTESIAN_POINT('',(5.,33.,6.));
#13687=CARTESIAN_POINT('',(1.,33.,6.));
#13688=CARTESIAN_POINT('',(5.,33.,6.));
#13689=CARTESIAN_POINT('',(1.,33.,9.));
#13690=CARTESIAN_POINT('',(1.,33.,6.));
#13691=CARTESIAN_POINT('',(5.,33.,9.));
#13692=CARTESIAN_POINT('',(5.,33.,9.));
#13693=CARTESIAN_POINT('',(5.,33.,6.));
#13694=CARTESIAN_POINT('Origin',(5.,31.,6.));
#13695=CARTESIAN_POINT('',(5.,31.,6.));
#13696=CARTESIAN_POINT('',(5.,31.,6.));
#13697=CARTESIAN_POINT('',(5.,31.,9.));
#13698=CARTESIAN_POINT('',(5.,31.,9.));
#13699=CARTESIAN_POINT('',(5.,31.,6.));
#13700=CARTESIAN_POINT('Origin',(1.,31.,6.));
#13701=CARTESIAN_POINT('',(1.,31.,6.));
#13702=CARTESIAN_POINT('',(1.,31.,6.));
#13703=CARTESIAN_POINT('',(1.,31.,9.));
#13704=CARTESIAN_POINT('',(1.,31.,9.));
#13705=CARTESIAN_POINT('',(1.,31.,6.));
#13706=CARTESIAN_POINT('Origin',(1.,33.,6.));
#13707=CARTESIAN_POINT('',(1.,33.,6.));
#13708=CARTESIAN_POINT('',(1.,33.,9.));
#13709=CARTESIAN_POINT('Origin',(3.,32.,9.));
#13710=CARTESIAN_POINT('Origin',(3.,32.,6.));
#13711=CARTESIAN_POINT('',(0.,0.,0.));
#13712=CARTESIAN_POINT('',(0.,0.,0.));
#13713=CARTESIAN_POINT('',(0.,0.,0.));
#13714=CARTESIAN_POINT('',(0.,0.,0.));
#13715=CARTESIAN_POINT('',(0.,0.,0.));
#13716=CARTESIAN_POINT('',(0.,0.,0.));
#13717=CARTESIAN_POINT('',(0.,0.,0.));
#13718=CARTESIAN_POINT('',(0.,0.,0.));
#13719=CARTESIAN_POINT('',(0.,0.,0.));
#13720=CARTESIAN_POINT('',(3.,0.5,8.));
#13721=CARTESIAN_POINT('',(3.,-3.2,8.));
#13722=CARTESIAN_POINT('',(4.4,-2.,5.42));
#13723=CARTESIAN_POINT('',(4.4,-2.,6.9));
#13724=CARTESIAN_POINT('',(1.6,-2.,6.9));
#13725=CARTESIAN_POINT('',(1.6,-2.,5.42));
#13726=CARTESIAN_POINT('',(3.,29.5,8.));
#13727=CARTESIAN_POINT('',(0.,0.,0.));
#13728=CARTESIAN_POINT('',(3.,33.2,8.));
#13729=CARTESIAN_POINT('',(0.,0.,0.));
#13730=CARTESIAN_POINT('',(4.4,32.,5.42));
#13731=CARTESIAN_POINT('',(1.6,32.,6.9));
#13732=CARTESIAN_POINT('',(1.6,32.,5.42));
#13733=CARTESIAN_POINT('',(4.4,32.,6.9));
#13734=CARTESIAN_POINT('',(0.,0.,0.));
#13735=CARTESIAN_POINT('',(0.,0.,0.));
#13736=CARTESIAN_POINT('',(0.,0.,0.));
#13737=CARTESIAN_POINT('',(7.57244285714286,0.,0.));
#13738=CARTESIAN_POINT('',(15.1448857142857,0.,0.));
#13739=CARTESIAN_POINT('',(22.7173285714286,0.,0.));
#13740=CARTESIAN_POINT('',(30.2897714285714,0.,0.));
#13741=CARTESIAN_POINT('',(37.8622142857143,0.,0.));
#13742=CARTESIAN_POINT('',(45.4346571428571,0.,0.));
#13743=CARTESIAN_POINT('',(53.0071,0.,0.));
#13744=UNCERTAINTY_MEASURE_WITH_UNIT(LENGTH_MEASURE(0.001),#13822,
'DISTANCE_ACCURACY_VALUE',
'Maximum model space distance between geometric entities at asserted c
onnectivities');
#13745=UNCERTAINTY_MEASURE_WITH_UNIT(LENGTH_MEASURE(0.001),#13822,
'DISTANCE_ACCURACY_VALUE',
'Maximum model space distance between geometric entities at asserted c
onnectivities');
#13746=UNCERTAINTY_MEASURE_WITH_UNIT(LENGTH_MEASURE(0.001),#13822,
'DISTANCE_ACCURACY_VALUE',
'Maximum model space distance between geometric entities at asserted c
onnectivities');
#13747=UNCERTAINTY_MEASURE_WITH_UNIT(LENGTH_MEASURE(0.001),#13822,
'DISTANCE_ACCURACY_VALUE',
'Maximum model space distance between geometric entities at asserted c
onnectivities');
#13748=UNCERTAINTY_MEASURE_WITH_UNIT(LENGTH_MEASURE(0.001),#13822,
'DISTANCE_ACCURACY_VALUE',
'Maximum model space distance between geometric entities at asserted c
onnectivities');
#13749=UNCERTAINTY_MEASURE_WITH_UNIT(LENGTH_MEASURE(0.001),#13822,
'DISTANCE_ACCURACY_VALUE',
'Maximum model space distance between geometric entities at asserted c
onnectivities');
#13750=UNCERTAINTY_MEASURE_WITH_UNIT(LENGTH_MEASURE(0.001),#13822,
'DISTANCE_ACCURACY_VALUE',
'Maximum model space distance between geometric entities at asserted c
onnectivities');
#13751=UNCERTAINTY_MEASURE_WITH_UNIT(LENGTH_MEASURE(0.001),#13822,
'DISTANCE_ACCURACY_VALUE',
'Maximum model space distance between geometric entities at asserted c
onnectivities');
#13752=UNCERTAINTY_MEASURE_WITH_UNIT(LENGTH_MEASURE(0.001),#13822,
'DISTANCE_ACCURACY_VALUE',
'Maximum model space distance between geometric entities at asserted c
onnectivities');
#13753=UNCERTAINTY_MEASURE_WITH_UNIT(LENGTH_MEASURE(0.001),#13822,
'DISTANCE_ACCURACY_VALUE',
'Maximum model space distance between geometric entities at asserted c
onnectivities');
#13754=UNCERTAINTY_MEASURE_WITH_UNIT(LENGTH_MEASURE(0.001),#13822,
'DISTANCE_ACCURACY_VALUE',
'Maximum model space distance between geometric entities at asserted c
onnectivities');
#13755=UNCERTAINTY_MEASURE_WITH_UNIT(LENGTH_MEASURE(0.001),#13822,
'DISTANCE_ACCURACY_VALUE',
'Maximum model space distance between geometric entities at asserted c
onnectivities');
#13756=UNCERTAINTY_MEASURE_WITH_UNIT(LENGTH_MEASURE(0.001),#13822,
'DISTANCE_ACCURACY_VALUE',
'Maximum model space distance between geometric entities at asserted c
onnectivities');
#13757=UNCERTAINTY_MEASURE_WITH_UNIT(LENGTH_MEASURE(0.001),#13822,
'DISTANCE_ACCURACY_VALUE',
'Maximum model space distance between geometric entities at asserted c
onnectivities');
#13758=UNCERTAINTY_MEASURE_WITH_UNIT(LENGTH_MEASURE(0.001),#13822,
'DISTANCE_ACCURACY_VALUE',
'Maximum model space distance between geometric entities at asserted c
onnectivities');
#13759=UNCERTAINTY_MEASURE_WITH_UNIT(LENGTH_MEASURE(0.001),#13822,
'DISTANCE_ACCURACY_VALUE',
'Maximum model space distance between geometric entities at asserted c
onnectivities');
#13760=UNCERTAINTY_MEASURE_WITH_UNIT(LENGTH_MEASURE(0.001),#13822,
'DISTANCE_ACCURACY_VALUE',
'Maximum model space distance between geometric entities at asserted c
onnectivities');
#13761=UNCERTAINTY_MEASURE_WITH_UNIT(LENGTH_MEASURE(0.001),#13822,
'DISTANCE_ACCURACY_VALUE',
'Maximum model space distance between geometric entities at asserted c
onnectivities');
#13762=UNCERTAINTY_MEASURE_WITH_UNIT(LENGTH_MEASURE(0.001),#13822,
'DISTANCE_ACCURACY_VALUE',
'Maximum model space distance between geometric entities at asserted c
onnectivities');
#13763=UNCERTAINTY_MEASURE_WITH_UNIT(LENGTH_MEASURE(0.001),#13822,
'DISTANCE_ACCURACY_VALUE',
'Maximum model space distance between geometric entities at asserted c
onnectivities');
#13764=UNCERTAINTY_MEASURE_WITH_UNIT(LENGTH_MEASURE(0.001),#13822,
'DISTANCE_ACCURACY_VALUE',
'Maximum model space distance between geometric entities at asserted c
onnectivities');
#13765=UNCERTAINTY_MEASURE_WITH_UNIT(LENGTH_MEASURE(0.001),#13822,
'DISTANCE_ACCURACY_VALUE',
'Maximum model space distance between geometric entities at asserted c
onnectivities');
#13766=UNCERTAINTY_MEASURE_WITH_UNIT(LENGTH_MEASURE(0.001),#13822,
'DISTANCE_ACCURACY_VALUE',
'Maximum model space distance between geometric entities at asserted c
onnectivities');
#13767=UNCERTAINTY_MEASURE_WITH_UNIT(LENGTH_MEASURE(0.001),#13822,
'DISTANCE_ACCURACY_VALUE',
'Maximum model space distance between geometric entities at asserted c
onnectivities');
#13768=UNCERTAINTY_MEASURE_WITH_UNIT(LENGTH_MEASURE(0.001),#13822,
'DISTANCE_ACCURACY_VALUE',
'Maximum model space distance between geometric entities at asserted c
onnectivities');
#13769=UNCERTAINTY_MEASURE_WITH_UNIT(LENGTH_MEASURE(0.001),#13822,
'DISTANCE_ACCURACY_VALUE',
'Maximum model space distance between geometric entities at asserted c
onnectivities');
#13770=UNCERTAINTY_MEASURE_WITH_UNIT(LENGTH_MEASURE(0.001),#13822,
'DISTANCE_ACCURACY_VALUE',
'Maximum model space distance between geometric entities at asserted c
onnectivities');
#13771=UNCERTAINTY_MEASURE_WITH_UNIT(LENGTH_MEASURE(0.001),#13822,
'DISTANCE_ACCURACY_VALUE',
'Maximum model space distance between geometric entities at asserted c
onnectivities');
#13772=UNCERTAINTY_MEASURE_WITH_UNIT(LENGTH_MEASURE(0.001),#13822,
'DISTANCE_ACCURACY_VALUE',
'Maximum model space distance between geometric entities at asserted c
onnectivities');
#13773=UNCERTAINTY_MEASURE_WITH_UNIT(LENGTH_MEASURE(0.001),#13822,
'DISTANCE_ACCURACY_VALUE',
'Maximum model space distance between geometric entities at asserted c
onnectivities');
#13774=UNCERTAINTY_MEASURE_WITH_UNIT(LENGTH_MEASURE(0.001),#13822,
'DISTANCE_ACCURACY_VALUE',
'Maximum model space distance between geometric entities at asserted c
onnectivities');
#13775=UNCERTAINTY_MEASURE_WITH_UNIT(LENGTH_MEASURE(0.001),#13822,
'DISTANCE_ACCURACY_VALUE',
'Maximum model space distance between geometric entities at asserted c
onnectivities');
#13776=UNCERTAINTY_MEASURE_WITH_UNIT(LENGTH_MEASURE(0.001),#13822,
'DISTANCE_ACCURACY_VALUE',
'Maximum model space distance between geometric entities at asserted c
onnectivities');
#13777=UNCERTAINTY_MEASURE_WITH_UNIT(LENGTH_MEASURE(0.001),#13822,
'DISTANCE_ACCURACY_VALUE',
'Maximum model space distance between geometric entities at asserted c
onnectivities');
#13778=UNCERTAINTY_MEASURE_WITH_UNIT(LENGTH_MEASURE(0.001),#13822,
'DISTANCE_ACCURACY_VALUE',
'Maximum model space distance between geometric entities at asserted c
onnectivities');
#13779=UNCERTAINTY_MEASURE_WITH_UNIT(LENGTH_MEASURE(0.001),#13822,
'DISTANCE_ACCURACY_VALUE',
'Maximum model space distance between geometric entities at asserted c
onnectivities');
#13780=UNCERTAINTY_MEASURE_WITH_UNIT(LENGTH_MEASURE(0.001),#13822,
'DISTANCE_ACCURACY_VALUE',
'Maximum model space distance between geometric entities at asserted c
onnectivities');
#13781=UNCERTAINTY_MEASURE_WITH_UNIT(LENGTH_MEASURE(0.001),#13822,
'DISTANCE_ACCURACY_VALUE',
'Maximum model space distance between geometric entities at asserted c
onnectivities');
#13782=UNCERTAINTY_MEASURE_WITH_UNIT(LENGTH_MEASURE(0.001),#13822,
'DISTANCE_ACCURACY_VALUE',
'Maximum model space distance between geometric entities at asserted c
onnectivities');
#13783=(
GEOMETRIC_REPRESENTATION_CONTEXT(3)
GLOBAL_UNCERTAINTY_ASSIGNED_CONTEXT((#13744))
GLOBAL_UNIT_ASSIGNED_CONTEXT((#13822,#13824,#13825))
REPRESENTATION_CONTEXT('','3D')
);
#13784=(
GEOMETRIC_REPRESENTATION_CONTEXT(3)
GLOBAL_UNCERTAINTY_ASSIGNED_CONTEXT((#13745))
GLOBAL_UNIT_ASSIGNED_CONTEXT((#13822,#13824,#13825))
REPRESENTATION_CONTEXT('','3D')
);
#13785=(
GEOMETRIC_REPRESENTATION_CONTEXT(3)
GLOBAL_UNCERTAINTY_ASSIGNED_CONTEXT((#13746))
GLOBAL_UNIT_ASSIGNED_CONTEXT((#13822,#13824,#13825))
REPRESENTATION_CONTEXT('','3D')
);
#13786=(
GEOMETRIC_REPRESENTATION_CONTEXT(3)
GLOBAL_UNCERTAINTY_ASSIGNED_CONTEXT((#13747))
GLOBAL_UNIT_ASSIGNED_CONTEXT((#13822,#13824,#13825))
REPRESENTATION_CONTEXT('','3D')
);
#13787=(
GEOMETRIC_REPRESENTATION_CONTEXT(3)
GLOBAL_UNCERTAINTY_ASSIGNED_CONTEXT((#13748))
GLOBAL_UNIT_ASSIGNED_CONTEXT((#13822,#13824,#13825))
REPRESENTATION_CONTEXT('','3D')
);
#13788=(
GEOMETRIC_REPRESENTATION_CONTEXT(3)
GLOBAL_UNCERTAINTY_ASSIGNED_CONTEXT((#13749))
GLOBAL_UNIT_ASSIGNED_CONTEXT((#13822,#13824,#13825))
REPRESENTATION_CONTEXT('','3D')
);
#13789=(
GEOMETRIC_REPRESENTATION_CONTEXT(3)
GLOBAL_UNCERTAINTY_ASSIGNED_CONTEXT((#13750))
GLOBAL_UNIT_ASSIGNED_CONTEXT((#13822,#13824,#13825))
REPRESENTATION_CONTEXT('','3D')
);
#13790=(
GEOMETRIC_REPRESENTATION_CONTEXT(3)
GLOBAL_UNCERTAINTY_ASSIGNED_CONTEXT((#13751))
GLOBAL_UNIT_ASSIGNED_CONTEXT((#13822,#13824,#13825))
REPRESENTATION_CONTEXT('','3D')
);
#13791=(
GEOMETRIC_REPRESENTATION_CONTEXT(3)
GLOBAL_UNCERTAINTY_ASSIGNED_CONTEXT((#13752))
GLOBAL_UNIT_ASSIGNED_CONTEXT((#13822,#13824,#13825))
REPRESENTATION_CONTEXT('','3D')
);
#13792=(
GEOMETRIC_REPRESENTATION_CONTEXT(3)
GLOBAL_UNCERTAINTY_ASSIGNED_CONTEXT((#13753))
GLOBAL_UNIT_ASSIGNED_CONTEXT((#13822,#13824,#13825))
REPRESENTATION_CONTEXT('','3D')
);
#13793=(
GEOMETRIC_REPRESENTATION_CONTEXT(3)
GLOBAL_UNCERTAINTY_ASSIGNED_CONTEXT((#13754))
GLOBAL_UNIT_ASSIGNED_CONTEXT((#13822,#13824,#13825))
REPRESENTATION_CONTEXT('','3D')
);
#13794=(
GEOMETRIC_REPRESENTATION_CONTEXT(3)
GLOBAL_UNCERTAINTY_ASSIGNED_CONTEXT((#13755))
GLOBAL_UNIT_ASSIGNED_CONTEXT((#13822,#13824,#13825))
REPRESENTATION_CONTEXT('','3D')
);
#13795=(
GEOMETRIC_REPRESENTATION_CONTEXT(3)
GLOBAL_UNCERTAINTY_ASSIGNED_CONTEXT((#13756))
GLOBAL_UNIT_ASSIGNED_CONTEXT((#13822,#13824,#13825))
REPRESENTATION_CONTEXT('','3D')
);
#13796=(
GEOMETRIC_REPRESENTATION_CONTEXT(3)
GLOBAL_UNCERTAINTY_ASSIGNED_CONTEXT((#13757))
GLOBAL_UNIT_ASSIGNED_CONTEXT((#13822,#13824,#13825))
REPRESENTATION_CONTEXT('','3D')
);
#13797=(
GEOMETRIC_REPRESENTATION_CONTEXT(3)
GLOBAL_UNCERTAINTY_ASSIGNED_CONTEXT((#13758))
GLOBAL_UNIT_ASSIGNED_CONTEXT((#13822,#13824,#13825))
REPRESENTATION_CONTEXT('','3D')
);
#13798=(
GEOMETRIC_REPRESENTATION_CONTEXT(3)
GLOBAL_UNCERTAINTY_ASSIGNED_CONTEXT((#13759))
GLOBAL_UNIT_ASSIGNED_CONTEXT((#13822,#13824,#13825))
REPRESENTATION_CONTEXT('','3D')
);
#13799=(
GEOMETRIC_REPRESENTATION_CONTEXT(3)
GLOBAL_UNCERTAINTY_ASSIGNED_CONTEXT((#13760))
GLOBAL_UNIT_ASSIGNED_CONTEXT((#13822,#13824,#13825))
REPRESENTATION_CONTEXT('','3D')
);
#13800=(
GEOMETRIC_REPRESENTATION_CONTEXT(3)
GLOBAL_UNCERTAINTY_ASSIGNED_CONTEXT((#13761))
GLOBAL_UNIT_ASSIGNED_CONTEXT((#13822,#13824,#13825))
REPRESENTATION_CONTEXT('','3D')
);
#13801=(
GEOMETRIC_REPRESENTATION_CONTEXT(3)
GLOBAL_UNCERTAINTY_ASSIGNED_CONTEXT((#13762))
GLOBAL_UNIT_ASSIGNED_CONTEXT((#13822,#13824,#13825))
REPRESENTATION_CONTEXT('','3D')
);
#13802=(
GEOMETRIC_REPRESENTATION_CONTEXT(3)
GLOBAL_UNCERTAINTY_ASSIGNED_CONTEXT((#13763))
GLOBAL_UNIT_ASSIGNED_CONTEXT((#13822,#13824,#13825))
REPRESENTATION_CONTEXT('','3D')
);
#13803=(
GEOMETRIC_REPRESENTATION_CONTEXT(3)
GLOBAL_UNCERTAINTY_ASSIGNED_CONTEXT((#13764))
GLOBAL_UNIT_ASSIGNED_CONTEXT((#13822,#13824,#13825))
REPRESENTATION_CONTEXT('','3D')
);
#13804=(
GEOMETRIC_REPRESENTATION_CONTEXT(3)
GLOBAL_UNCERTAINTY_ASSIGNED_CONTEXT((#13765))
GLOBAL_UNIT_ASSIGNED_CONTEXT((#13822,#13824,#13825))
REPRESENTATION_CONTEXT('','3D')
);
#13805=(
GEOMETRIC_REPRESENTATION_CONTEXT(3)
GLOBAL_UNCERTAINTY_ASSIGNED_CONTEXT((#13766))
GLOBAL_UNIT_ASSIGNED_CONTEXT((#13822,#13824,#13825))
REPRESENTATION_CONTEXT('','3D')
);
#13806=(
GEOMETRIC_REPRESENTATION_CONTEXT(3)
GLOBAL_UNCERTAINTY_ASSIGNED_CONTEXT((#13767))
GLOBAL_UNIT_ASSIGNED_CONTEXT((#13822,#13824,#13825))
REPRESENTATION_CONTEXT('','3D')
);
#13807=(
GEOMETRIC_REPRESENTATION_CONTEXT(3)
GLOBAL_UNCERTAINTY_ASSIGNED_CONTEXT((#13768))
GLOBAL_UNIT_ASSIGNED_CONTEXT((#13822,#13824,#13825))
REPRESENTATION_CONTEXT('','3D')
);
#13808=(
GEOMETRIC_REPRESENTATION_CONTEXT(3)
GLOBAL_UNCERTAINTY_ASSIGNED_CONTEXT((#13769))
GLOBAL_UNIT_ASSIGNED_CONTEXT((#13822,#13824,#13825))
REPRESENTATION_CONTEXT('','3D')
);
#13809=(
GEOMETRIC_REPRESENTATION_CONTEXT(3)
GLOBAL_UNCERTAINTY_ASSIGNED_CONTEXT((#13770))
GLOBAL_UNIT_ASSIGNED_CONTEXT((#13822,#13824,#13825))
REPRESENTATION_CONTEXT('','3D')
);
#13810=(
GEOMETRIC_REPRESENTATION_CONTEXT(3)
GLOBAL_UNCERTAINTY_ASSIGNED_CONTEXT((#13771))
GLOBAL_UNIT_ASSIGNED_CONTEXT((#13822,#13824,#13825))
REPRESENTATION_CONTEXT('','3D')
);
#13811=(
GEOMETRIC_REPRESENTATION_CONTEXT(3)
GLOBAL_UNCERTAINTY_ASSIGNED_CONTEXT((#13772))
GLOBAL_UNIT_ASSIGNED_CONTEXT((#13822,#13824,#13825))
REPRESENTATION_CONTEXT('','3D')
);
#13812=(
GEOMETRIC_REPRESENTATION_CONTEXT(3)
GLOBAL_UNCERTAINTY_ASSIGNED_CONTEXT((#13773))
GLOBAL_UNIT_ASSIGNED_CONTEXT((#13822,#13824,#13825))
REPRESENTATION_CONTEXT('','3D')
);
#13813=(
GEOMETRIC_REPRESENTATION_CONTEXT(3)
GLOBAL_UNCERTAINTY_ASSIGNED_CONTEXT((#13774))
GLOBAL_UNIT_ASSIGNED_CONTEXT((#13822,#13824,#13825))
REPRESENTATION_CONTEXT('','3D')
);
#13814=(
GEOMETRIC_REPRESENTATION_CONTEXT(3)
GLOBAL_UNCERTAINTY_ASSIGNED_CONTEXT((#13775))
GLOBAL_UNIT_ASSIGNED_CONTEXT((#13822,#13824,#13825))
REPRESENTATION_CONTEXT('','3D')
);
#13815=(
GEOMETRIC_REPRESENTATION_CONTEXT(3)
GLOBAL_UNCERTAINTY_ASSIGNED_CONTEXT((#13776))
GLOBAL_UNIT_ASSIGNED_CONTEXT((#13822,#13824,#13825))
REPRESENTATION_CONTEXT('','3D')
);
#13816=(
GEOMETRIC_REPRESENTATION_CONTEXT(3)
GLOBAL_UNCERTAINTY_ASSIGNED_CONTEXT((#13777))
GLOBAL_UNIT_ASSIGNED_CONTEXT((#13822,#13824,#13825))
REPRESENTATION_CONTEXT('','3D')
);
#13817=(
GEOMETRIC_REPRESENTATION_CONTEXT(3)
GLOBAL_UNCERTAINTY_ASSIGNED_CONTEXT((#13778))
GLOBAL_UNIT_ASSIGNED_CONTEXT((#13822,#13824,#13825))
REPRESENTATION_CONTEXT('','3D')
);
#13818=(
GEOMETRIC_REPRESENTATION_CONTEXT(3)
GLOBAL_UNCERTAINTY_ASSIGNED_CONTEXT((#13779))
GLOBAL_UNIT_ASSIGNED_CONTEXT((#13822,#13824,#13825))
REPRESENTATION_CONTEXT('','3D')
);
#13819=(
GEOMETRIC_REPRESENTATION_CONTEXT(3)
GLOBAL_UNCERTAINTY_ASSIGNED_CONTEXT((#13780))
GLOBAL_UNIT_ASSIGNED_CONTEXT((#13822,#13824,#13825))
REPRESENTATION_CONTEXT('','3D')
);
#13820=(
GEOMETRIC_REPRESENTATION_CONTEXT(3)
GLOBAL_UNCERTAINTY_ASSIGNED_CONTEXT((#13781))
GLOBAL_UNIT_ASSIGNED_CONTEXT((#13822,#13824,#13825))
REPRESENTATION_CONTEXT('','3D')
);
#13821=(
GEOMETRIC_REPRESENTATION_CONTEXT(3)
GLOBAL_UNCERTAINTY_ASSIGNED_CONTEXT((#13782))
GLOBAL_UNIT_ASSIGNED_CONTEXT((#13822,#13824,#13825))
REPRESENTATION_CONTEXT('','3D')
);
#13822=(
LENGTH_UNIT()
NAMED_UNIT(*)
SI_UNIT(.CENTI.,.METRE.)
);
#13823=(
LENGTH_UNIT()
NAMED_UNIT(*)
SI_UNIT($,.METRE.)
);
#13824=(
NAMED_UNIT(*)
PLANE_ANGLE_UNIT()
SI_UNIT($,.RADIAN.)
);
#13825=(
NAMED_UNIT(*)
SI_UNIT($,.STERADIAN.)
SOLID_ANGLE_UNIT()
);
#13826=SHAPE_DEFINITION_REPRESENTATION(#13864,#13996);
#13827=SHAPE_DEFINITION_REPRESENTATION(#13865,#13997);
#13828=SHAPE_DEFINITION_REPRESENTATION(#13866,#13998);
#13829=SHAPE_DEFINITION_REPRESENTATION(#13867,#13999);
#13830=SHAPE_DEFINITION_REPRESENTATION(#13868,#14000);
#13831=SHAPE_DEFINITION_REPRESENTATION(#13869,#14001);
#13832=SHAPE_DEFINITION_REPRESENTATION(#13870,#14002);
#13833=SHAPE_DEFINITION_REPRESENTATION(#13871,#14003);
#13834=SHAPE_DEFINITION_REPRESENTATION(#13872,#14004);
#13835=SHAPE_DEFINITION_REPRESENTATION(#13873,#14005);
#13836=SHAPE_DEFINITION_REPRESENTATION(#13874,#14006);
#13837=SHAPE_DEFINITION_REPRESENTATION(#13875,#14007);
#13838=SHAPE_DEFINITION_REPRESENTATION(#13876,#14008);
#13839=SHAPE_DEFINITION_REPRESENTATION(#13877,#14009);
#13840=SHAPE_DEFINITION_REPRESENTATION(#13878,#14010);
#13841=SHAPE_DEFINITION_REPRESENTATION(#13879,#14011);
#13842=SHAPE_DEFINITION_REPRESENTATION(#13880,#14012);
#13843=SHAPE_DEFINITION_REPRESENTATION(#13881,#14013);
#13844=SHAPE_DEFINITION_REPRESENTATION(#13882,#14014);
#13845=SHAPE_DEFINITION_REPRESENTATION(#13883,#14015);
#13846=SHAPE_DEFINITION_REPRESENTATION(#13884,#14016);
#13847=SHAPE_DEFINITION_REPRESENTATION(#13885,#14017);
#13848=SHAPE_DEFINITION_REPRESENTATION(#13886,#14018);
#13849=SHAPE_DEFINITION_REPRESENTATION(#13887,#14019);
#13850=SHAPE_DEFINITION_REPRESENTATION(#13888,#14020);
#13851=SHAPE_DEFINITION_REPRESENTATION(#13889,#14021);
#13852=SHAPE_DEFINITION_REPRESENTATION(#13890,#14022);
#13853=SHAPE_DEFINITION_REPRESENTATION(#13891,#14023);
#13854=SHAPE_DEFINITION_REPRESENTATION(#13892,#14024);
#13855=SHAPE_DEFINITION_REPRESENTATION(#13893,#14025);
#13856=SHAPE_DEFINITION_REPRESENTATION(#13894,#14026);
#13857=SHAPE_DEFINITION_REPRESENTATION(#13895,#14027);
#13858=SHAPE_DEFINITION_REPRESENTATION(#13901,#14028);
#13859=SHAPE_DEFINITION_REPRESENTATION(#13902,#14029);
#13860=SHAPE_DEFINITION_REPRESENTATION(#13903,#14030);
#13861=SHAPE_DEFINITION_REPRESENTATION(#13904,#14031);
#13862=SHAPE_DEFINITION_REPRESENTATION(#13905,#14032);
#13863=SHAPE_DEFINITION_REPRESENTATION(#13962,#14033);
#13864=PRODUCT_DEFINITION_SHAPE('',$,#14035);
#13865=PRODUCT_DEFINITION_SHAPE('',$,#14036);
#13866=PRODUCT_DEFINITION_SHAPE('',$,#14037);
#13867=PRODUCT_DEFINITION_SHAPE('',$,#14038);
#13868=PRODUCT_DEFINITION_SHAPE('',$,#14039);
#13869=PRODUCT_DEFINITION_SHAPE('',$,#14040);
#13870=PRODUCT_DEFINITION_SHAPE('',$,#14041);
#13871=PRODUCT_DEFINITION_SHAPE('',$,#14042);
#13872=PRODUCT_DEFINITION_SHAPE('',$,#14043);
#13873=PRODUCT_DEFINITION_SHAPE('',$,#14044);
#13874=PRODUCT_DEFINITION_SHAPE('',$,#14045);
#13875=PRODUCT_DEFINITION_SHAPE('',$,#14046);
#13876=PRODUCT_DEFINITION_SHAPE('',$,#14047);
#13877=PRODUCT_DEFINITION_SHAPE('',$,#14048);
#13878=PRODUCT_DEFINITION_SHAPE('',$,#14049);
#13879=PRODUCT_DEFINITION_SHAPE('',$,#14050);
#13880=PRODUCT_DEFINITION_SHAPE('',$,#14051);
#13881=PRODUCT_DEFINITION_SHAPE('',$,#14052);
#13882=PRODUCT_DEFINITION_SHAPE('',$,#14053);
#13883=PRODUCT_DEFINITION_SHAPE('',$,#14054);
#13884=PRODUCT_DEFINITION_SHAPE('',$,#14055);
#13885=PRODUCT_DEFINITION_SHAPE('',$,#14056);
#13886=PRODUCT_DEFINITION_SHAPE('',$,#14057);
#13887=PRODUCT_DEFINITION_SHAPE('',$,#14058);
#13888=PRODUCT_DEFINITION_SHAPE('',$,#14059);
#13889=PRODUCT_DEFINITION_SHAPE('',$,#14060);
#13890=PRODUCT_DEFINITION_SHAPE('',$,#14061);
#13891=PRODUCT_DEFINITION_SHAPE('',$,#14062);
#13892=PRODUCT_DEFINITION_SHAPE('',$,#14063);
#13893=PRODUCT_DEFINITION_SHAPE('',$,#14064);
#13894=PRODUCT_DEFINITION_SHAPE('',$,#14065);
#13895=PRODUCT_DEFINITION_SHAPE('',$,#14066);
#13896=PRODUCT_DEFINITION_SHAPE($,$,#295);
#13897=PRODUCT_DEFINITION_SHAPE($,$,#296);
#13898=PRODUCT_DEFINITION_SHAPE($,$,#297);
#13899=PRODUCT_DEFINITION_SHAPE($,$,#298);
#13900=PRODUCT_DEFINITION_SHAPE($,$,#299);
#13901=PRODUCT_DEFINITION_SHAPE('',$,#14067);
#13902=PRODUCT_DEFINITION_SHAPE('',$,#14068);
#13903=PRODUCT_DEFINITION_SHAPE('',$,#14069);
#13904=PRODUCT_DEFINITION_SHAPE('',$,#14070);
#13905=PRODUCT_DEFINITION_SHAPE('',$,#14071);
#13906=PRODUCT_DEFINITION_SHAPE($,$,#300);
#13907=PRODUCT_DEFINITION_SHAPE($,$,#301);
#13908=PRODUCT_DEFINITION_SHAPE($,$,#302);
#13909=PRODUCT_DEFINITION_SHAPE($,$,#303);
#13910=PRODUCT_DEFINITION_SHAPE($,$,#304);
#13911=PRODUCT_DEFINITION_SHAPE($,$,#305);
#13912=PRODUCT_DEFINITION_SHAPE($,$,#306);
#13913=PRODUCT_DEFINITION_SHAPE($,$,#307);
#13914=PRODUCT_DEFINITION_SHAPE($,$,#308);
#13915=PRODUCT_DEFINITION_SHAPE($,$,#309);
#13916=PRODUCT_DEFINITION_SHAPE($,$,#310);
#13917=PRODUCT_DEFINITION_SHAPE($,$,#311);
#13918=PRODUCT_DEFINITION_SHAPE($,$,#312);
#13919=PRODUCT_DEFINITION_SHAPE($,$,#313);
#13920=PRODUCT_DEFINITION_SHAPE($,$,#314);
#13921=PRODUCT_DEFINITION_SHAPE($,$,#315);
#13922=PRODUCT_DEFINITION_SHAPE($,$,#316);
#13923=PRODUCT_DEFINITION_SHAPE($,$,#317);
#13924=PRODUCT_DEFINITION_SHAPE($,$,#318);
#13925=PRODUCT_DEFINITION_SHAPE($,$,#319);
#13926=PRODUCT_DEFINITION_SHAPE($,$,#320);
#13927=PRODUCT_DEFINITION_SHAPE($,$,#321);
#13928=PRODUCT_DEFINITION_SHAPE($,$,#322);
#13929=PRODUCT_DEFINITION_SHAPE($,$,#323);
#13930=PRODUCT_DEFINITION_SHAPE($,$,#324);
#13931=PRODUCT_DEFINITION_SHAPE($,$,#325);
#13932=PRODUCT_DEFINITION_SHAPE($,$,#326);
#13933=PRODUCT_DEFINITION_SHAPE($,$,#327);
#13934=PRODUCT_DEFINITION_SHAPE($,$,#328);
#13935=PRODUCT_DEFINITION_SHAPE($,$,#329);
#13936=PRODUCT_DEFINITION_SHAPE($,$,#330);
#13937=PRODUCT_DEFINITION_SHAPE($,$,#331);
#13938=PRODUCT_DEFINITION_SHAPE($,$,#332);
#13939=PRODUCT_DEFINITION_SHAPE($,$,#333);
#13940=PRODUCT_DEFINITION_SHAPE($,$,#334);
#13941=PRODUCT_DEFINITION_SHAPE($,$,#335);
#13942=PRODUCT_DEFINITION_SHAPE($,$,#336);
#13943=PRODUCT_DEFINITION_SHAPE($,$,#337);
#13944=PRODUCT_DEFINITION_SHAPE($,$,#338);
#13945=PRODUCT_DEFINITION_SHAPE($,$,#339);
#13946=PRODUCT_DEFINITION_SHAPE($,$,#340);
#13947=PRODUCT_DEFINITION_SHAPE($,$,#341);
#13948=PRODUCT_DEFINITION_SHAPE($,$,#342);
#13949=PRODUCT_DEFINITION_SHAPE($,$,#343);
#13950=PRODUCT_DEFINITION_SHAPE($,$,#344);
#13951=PRODUCT_DEFINITION_SHAPE($,$,#345);
#13952=PRODUCT_DEFINITION_SHAPE($,$,#346);
#13953=PRODUCT_DEFINITION_SHAPE($,$,#347);
#13954=PRODUCT_DEFINITION_SHAPE($,$,#348);
#13955=PRODUCT_DEFINITION_SHAPE($,$,#349);
#13956=PRODUCT_DEFINITION_SHAPE($,$,#350);
#13957=PRODUCT_DEFINITION_SHAPE($,$,#351);
#13958=PRODUCT_DEFINITION_SHAPE($,$,#352);
#13959=PRODUCT_DEFINITION_SHAPE($,$,#353);
#13960=PRODUCT_DEFINITION_SHAPE($,$,#354);
#13961=PRODUCT_DEFINITION_SHAPE($,$,#355);
#13962=PRODUCT_DEFINITION_SHAPE('',$,#14072);
#13963=PRODUCT_DEFINITION_SHAPE($,$,#356);
#13964=PRODUCT_DEFINITION_SHAPE($,$,#357);
#13965=PRODUCT_DEFINITION_SHAPE($,$,#358);
#13966=PRODUCT_DEFINITION_SHAPE($,$,#359);
#13967=PRODUCT_DEFINITION_SHAPE($,$,#360);
#13968=PRODUCT_DEFINITION_SHAPE($,$,#361);
#13969=PRODUCT_DEFINITION_SHAPE($,$,#362);
#13970=PRODUCT_DEFINITION_SHAPE($,$,#363);
#13971=PRODUCT_DEFINITION_SHAPE($,$,#364);
#13972=PRODUCT_DEFINITION_SHAPE($,$,#365);
#13973=PRODUCT_DEFINITION_SHAPE($,$,#366);
#13974=PRODUCT_DEFINITION_SHAPE($,$,#367);
#13975=PRODUCT_DEFINITION_SHAPE($,$,#368);
#13976=PRODUCT_DEFINITION_SHAPE($,$,#369);
#13977=PRODUCT_DEFINITION_SHAPE($,$,#370);
#13978=PRODUCT_DEFINITION_SHAPE($,$,#371);
#13979=PRODUCT_DEFINITION_SHAPE($,$,#372);
#13980=PRODUCT_DEFINITION_SHAPE($,$,#373);
#13981=PRODUCT_DEFINITION_SHAPE($,$,#374);
#13982=PRODUCT_DEFINITION_SHAPE($,$,#375);
#13983=PRODUCT_DEFINITION_SHAPE($,$,#376);
#13984=PRODUCT_DEFINITION_SHAPE($,$,#377);
#13985=PRODUCT_DEFINITION_SHAPE($,$,#378);
#13986=PRODUCT_DEFINITION_SHAPE($,$,#379);
#13987=PRODUCT_DEFINITION_SHAPE($,$,#380);
#13988=PRODUCT_DEFINITION_SHAPE($,$,#381);
#13989=PRODUCT_DEFINITION_SHAPE($,$,#382);
#13990=PRODUCT_DEFINITION_SHAPE($,$,#383);
#13991=PRODUCT_DEFINITION_SHAPE($,$,#384);
#13992=PRODUCT_DEFINITION_SHAPE($,$,#385);
#13993=PRODUCT_DEFINITION_SHAPE($,$,#386);
#13994=PRODUCT_DEFINITION_SHAPE($,$,#387);
#13995=PRODUCT_DEFINITION_SHAPE($,$,#388);
#13996=SHAPE_REPRESENTATION('',(#8048,#8808,#8809,#8810,#8811,#8812,#8813,
#8814,#8815,#8816),#13783);
#13997=SHAPE_REPRESENTATION('',(#8049,#8704,#8705,#8706,#8707,#8708,#8709,
#8710,#8711,#8712,#8713,#8714,#8715,#8716,#8717,#8718,#8719,#8720,#8721,
#8722,#8723,#8724,#8725,#8726,#8727,#8728,#8729,#8730,#8731,#8732,#8733,
#8734,#8735,#8736,#8737,#8738,#8739,#8740,#8741,#8742,#8743,#8744,#8745,
#8746,#8747,#8748,#8749,#8750,#8751,#8752,#8753,#8754,#8755,#8756,#8757,
#8758,#8759),#13784);
#13998=SHAPE_REPRESENTATION('',(#8050),#13785);
#13999=SHAPE_REPRESENTATION('',(#8069),#13786);
#14000=SHAPE_REPRESENTATION('',(#8123),#13787);
#14001=SHAPE_REPRESENTATION('',(#8177),#13788);
#14002=SHAPE_REPRESENTATION('',(#8227),#13789);
#14003=SHAPE_REPRESENTATION('',(#8255),#13790);
#14004=SHAPE_REPRESENTATION('',(#8281),#13791);
#14005=SHAPE_REPRESENTATION('',(#8300),#13792);
#14006=SHAPE_REPRESENTATION('',(#8311),#13793);
#14007=SHAPE_REPRESENTATION('',(#8324),#13794);
#14008=SHAPE_REPRESENTATION('',(#8331),#13795);
#14009=SHAPE_REPRESENTATION('',(#8338),#13796);
#14010=SHAPE_REPRESENTATION('',(#8351),#13797);
#14011=SHAPE_REPRESENTATION('',(#8358),#13798);
#14012=SHAPE_REPRESENTATION('',(#8365,#8784,#8785,#8786,#8787,#8788,#8789,
#8790,#8791,#8792,#8793,#8794,#8795,#8796,#8797,#8798,#8799,#8800,#8801,
#8802,#8803,#8804,#8805,#8806,#8807),#13799);
#14013=SHAPE_REPRESENTATION('',(#8366),#13800);
#14014=SHAPE_REPRESENTATION('',(#8375),#13801);
#14015=SHAPE_REPRESENTATION('',(#8388),#13802);
#14016=SHAPE_REPRESENTATION('',(#8401),#13803);
#14017=SHAPE_REPRESENTATION('',(#8414),#13804);
#14018=SHAPE_REPRESENTATION('',(#8427),#13805);
#14019=SHAPE_REPRESENTATION('',(#8441),#13806);
#14020=SHAPE_REPRESENTATION('',(#8465),#13807);
#14021=SHAPE_REPRESENTATION('',(#8474),#13808);
#14022=SHAPE_REPRESENTATION('',(#8483,#8612,#8613,#8614,#8615,#8616),#13809);
#14023=SHAPE_REPRESENTATION('',(#8484),#13810);
#14024=SHAPE_REPRESENTATION('',(#8504),#13811);
#14025=SHAPE_REPRESENTATION('',(#8524),#13812);
#14026=SHAPE_REPRESENTATION('',(#8541),#13813);
#14027=SHAPE_REPRESENTATION('',(#8595),#13814);
#14028=SHAPE_REPRESENTATION('',(#8617),#13815);
#14029=SHAPE_REPRESENTATION('',(#8626),#13816);
#14030=SHAPE_REPRESENTATION('',(#8650),#13817);
#14031=SHAPE_REPRESENTATION('',(#8659),#13818);
#14032=SHAPE_REPRESENTATION('',(#8680),#13819);
#14033=SHAPE_REPRESENTATION('',(#8760),#13820);
#14034=PRODUCT_DEFINITION_CONTEXT('part definition',#14150,'design');
#14035=PRODUCT_DEFINITION('Gravity roller conveyor section',
'PAT-047',#14073,#14034);
#14036=PRODUCT_DEFINITION('Conveyor frame','Conveyor frame',#14074,#14034);
#14037=PRODUCT_DEFINITION('Rail splice plate','Rail splice plate',#14075,
#14034);
#14038=PRODUCT_DEFINITION('Drilled 400 mm rail','Drilled 400 mm rail',#14076,
#14034);
#14039=PRODUCT_DEFINITION('Drilled 200 mm rail','Drilled 200 mm rail',#14077,
#14034);
#14040=PRODUCT_DEFINITION('Slotted Extrusion - 20 x 20 x 200 mm',
'Slotted Extrusion - 20 x 20 x 200 mm',#14078,#14034);
#14041=PRODUCT_DEFINITION('M5x40 leg screw','M5x40 leg screw',#14079,#14034);
#14042=PRODUCT_DEFINITION('Cap Screw - M5x20','Cap Screw - M5x20',#14080,
#14034);
#14043=PRODUCT_DEFINITION('Rail splice plate_1','Rail splice plate (1)',
#14081,#14034);
#14044=PRODUCT_DEFINITION('Flat Washer - M5','Flat Washer - M5',#14082,
#14034);
#14045=PRODUCT_DEFINITION('Cross foot','Cross foot',#14083,#14034);
#14046=PRODUCT_DEFINITION('Bonded foot pad','Bonded foot pad',#14084,#14034);
#14047=PRODUCT_DEFINITION('Bonded foot pad_1','Bonded foot pad (1)',#14085,
#14034);
#14048=PRODUCT_DEFINITION('Cross foot_1','Cross foot (1)',#14086,#14034);
#14049=PRODUCT_DEFINITION('Bonded foot pad_2','Bonded foot pad (2)',#14087,
#14034);
#14050=PRODUCT_DEFINITION('Bonded foot pad_3','Bonded foot pad (3)',#14088,
#14034);
#14051=PRODUCT_DEFINITION('Roller 1','Roller 1',#14089,#14034);
#14052=PRODUCT_DEFINITION('Roller tube','Roller tube',#14090,#14034);
#14053=PRODUCT_DEFINITION('Bearing insert','Bearing insert',#14091,#14034);
#14054=PRODUCT_DEFINITION('Bearing retainer','Bearing retainer',#14092,
#14034);
#14055=PRODUCT_DEFINITION('Bearing insert_1','Bearing insert (1)',#14093,
#14034);
#14056=PRODUCT_DEFINITION('Bearing retainer_1','Bearing retainer (1)',#14094,
#14034);
#14057=PRODUCT_DEFINITION('Dead axle','Dead axle',#14095,#14034);
#14058=PRODUCT_DEFINITION('Axle support','Axle support',#14096,#14034);
#14059=PRODUCT_DEFINITION('Axle keeper','Axle keeper',#14097,#14034);
#14060=PRODUCT_DEFINITION('Inner race spacer','Inner race spacer',#14098,
#14034);
#14061=PRODUCT_DEFINITION('Sealed Ball Bearing - 10 x 30 x 9 mm',
'Sealed Ball Bearing - 10 x 30 x 9 mm',#14099,#14034);
#14062=PRODUCT_DEFINITION('Inner ring','Inner ring',#14100,#14034);
#14063=PRODUCT_DEFINITION('Outer ring','Outer ring',#14101,#14034);
#14064=PRODUCT_DEFINITION('Balls','Balls',#14102,#14034);
#14065=PRODUCT_DEFINITION('Cage','Cage',#14103,#14034);
#14066=PRODUCT_DEFINITION('Seals 2RS','Seals 2RS',#14104,#14034);
#14067=PRODUCT_DEFINITION('Inner race spacer_1','Inner race spacer (1)',
#14105,#14034);
#14068=PRODUCT_DEFINITION('M4x10 Cap Screw','M4x10 Cap Screw',#14106,#14034);
#14069=PRODUCT_DEFINITION('Axle keeper_1','Axle keeper (1)',#14107,#14034);
#14070=PRODUCT_DEFINITION('Captive slot nut','Captive slot nut',#14108,
#14034);
#14071=PRODUCT_DEFINITION('M5x14 Cap Screw','M5x14 Cap Screw',#14109,#14034);
#14072=PRODUCT_DEFINITION('Axle support_1','Axle support (1)',#14110,#14034);
#14073=PRODUCT_DEFINITION_FORMATION('',$,#14152);
#14074=PRODUCT_DEFINITION_FORMATION('',$,#14153);
#14075=PRODUCT_DEFINITION_FORMATION('',$,#14154);
#14076=PRODUCT_DEFINITION_FORMATION('',$,#14155);
#14077=PRODUCT_DEFINITION_FORMATION('',$,#14156);
#14078=PRODUCT_DEFINITION_FORMATION('',$,#14157);
#14079=PRODUCT_DEFINITION_FORMATION('',$,#14158);
#14080=PRODUCT_DEFINITION_FORMATION('',$,#14159);
#14081=PRODUCT_DEFINITION_FORMATION('',$,#14160);
#14082=PRODUCT_DEFINITION_FORMATION('',$,#14161);
#14083=PRODUCT_DEFINITION_FORMATION('',$,#14162);
#14084=PRODUCT_DEFINITION_FORMATION('',$,#14163);
#14085=PRODUCT_DEFINITION_FORMATION('',$,#14164);
#14086=PRODUCT_DEFINITION_FORMATION('',$,#14165);
#14087=PRODUCT_DEFINITION_FORMATION('',$,#14166);
#14088=PRODUCT_DEFINITION_FORMATION('',$,#14167);
#14089=PRODUCT_DEFINITION_FORMATION('',$,#14168);
#14090=PRODUCT_DEFINITION_FORMATION('',$,#14169);
#14091=PRODUCT_DEFINITION_FORMATION('',$,#14170);
#14092=PRODUCT_DEFINITION_FORMATION('',$,#14171);
#14093=PRODUCT_DEFINITION_FORMATION('',$,#14172);
#14094=PRODUCT_DEFINITION_FORMATION('',$,#14173);
#14095=PRODUCT_DEFINITION_FORMATION('',$,#14174);
#14096=PRODUCT_DEFINITION_FORMATION('',$,#14175);
#14097=PRODUCT_DEFINITION_FORMATION('',$,#14176);
#14098=PRODUCT_DEFINITION_FORMATION('',$,#14177);
#14099=PRODUCT_DEFINITION_FORMATION('',$,#14178);
#14100=PRODUCT_DEFINITION_FORMATION('',$,#14179);
#14101=PRODUCT_DEFINITION_FORMATION('',$,#14180);
#14102=PRODUCT_DEFINITION_FORMATION('',$,#14181);
#14103=PRODUCT_DEFINITION_FORMATION('',$,#14182);
#14104=PRODUCT_DEFINITION_FORMATION('',$,#14183);
#14105=PRODUCT_DEFINITION_FORMATION('',$,#14184);
#14106=PRODUCT_DEFINITION_FORMATION('',$,#14185);
#14107=PRODUCT_DEFINITION_FORMATION('',$,#14186);
#14108=PRODUCT_DEFINITION_FORMATION('',$,#14187);
#14109=PRODUCT_DEFINITION_FORMATION('',$,#14188);
#14110=PRODUCT_DEFINITION_FORMATION('',$,#14189);
#14111=PRODUCT_RELATED_PRODUCT_CATEGORY(
'PAT-047',
'PAT-047',(#14152));
#14112=PRODUCT_RELATED_PRODUCT_CATEGORY('Conveyor frame',
'Conveyor frame',(#14153));
#14113=PRODUCT_RELATED_PRODUCT_CATEGORY('Rail splice plate',
'Rail splice plate',(#14154));
#14114=PRODUCT_RELATED_PRODUCT_CATEGORY('Drilled 400 mm rail',
'Drilled 400 mm rail',(#14155));
#14115=PRODUCT_RELATED_PRODUCT_CATEGORY('Drilled 200 mm rail',
'Drilled 200 mm rail',(#14156));
#14116=PRODUCT_RELATED_PRODUCT_CATEGORY(
'Slotted Extrusion - 20 x 20 x 200 mm',
'Slotted Extrusion - 20 x 20 x 200 mm',(#14157));
#14117=PRODUCT_RELATED_PRODUCT_CATEGORY('M5x40 leg screw',
'M5x40 leg screw',(#14158));
#14118=PRODUCT_RELATED_PRODUCT_CATEGORY('Cap Screw - M5x20',
'Cap Screw - M5x20',(#14159));
#14119=PRODUCT_RELATED_PRODUCT_CATEGORY('Rail splice plate (1)',
'Rail splice plate (1)',(#14160));
#14120=PRODUCT_RELATED_PRODUCT_CATEGORY('Flat Washer - M5',
'Flat Washer - M5',(#14161));
#14121=PRODUCT_RELATED_PRODUCT_CATEGORY('Cross foot','Cross foot',(#14162));
#14122=PRODUCT_RELATED_PRODUCT_CATEGORY('Bonded foot pad',
'Bonded foot pad',(#14163));
#14123=PRODUCT_RELATED_PRODUCT_CATEGORY('Bonded foot pad (1)',
'Bonded foot pad (1)',(#14164));
#14124=PRODUCT_RELATED_PRODUCT_CATEGORY('Cross foot (1)',
'Cross foot (1)',(#14165));
#14125=PRODUCT_RELATED_PRODUCT_CATEGORY('Bonded foot pad (2)',
'Bonded foot pad (2)',(#14166));
#14126=PRODUCT_RELATED_PRODUCT_CATEGORY('Bonded foot pad (3)',
'Bonded foot pad (3)',(#14167));
#14127=PRODUCT_RELATED_PRODUCT_CATEGORY('Roller 1','Roller 1',(#14168));
#14128=PRODUCT_RELATED_PRODUCT_CATEGORY('Roller tube','Roller tube',(#14169));
#14129=PRODUCT_RELATED_PRODUCT_CATEGORY('Bearing insert',
'Bearing insert',(#14170));
#14130=PRODUCT_RELATED_PRODUCT_CATEGORY('Bearing retainer',
'Bearing retainer',(#14171));
#14131=PRODUCT_RELATED_PRODUCT_CATEGORY('Bearing insert (1)',
'Bearing insert (1)',(#14172));
#14132=PRODUCT_RELATED_PRODUCT_CATEGORY('Bearing retainer (1)',
'Bearing retainer (1)',(#14173));
#14133=PRODUCT_RELATED_PRODUCT_CATEGORY('Dead axle','Dead axle',(#14174));
#14134=PRODUCT_RELATED_PRODUCT_CATEGORY('Axle support','Axle support',(#14175));
#14135=PRODUCT_RELATED_PRODUCT_CATEGORY('Axle keeper','Axle keeper',(#14176));
#14136=PRODUCT_RELATED_PRODUCT_CATEGORY('Inner race spacer',
'Inner race spacer',(#14177));
#14137=PRODUCT_RELATED_PRODUCT_CATEGORY(
'Sealed Ball Bearing - 10 x 30 x 9 mm',
'Sealed Ball Bearing - 10 x 30 x 9 mm',(#14178));
#14138=PRODUCT_RELATED_PRODUCT_CATEGORY('Inner ring','Inner ring',(#14179));
#14139=PRODUCT_RELATED_PRODUCT_CATEGORY('Outer ring','Outer ring',(#14180));
#14140=PRODUCT_RELATED_PRODUCT_CATEGORY('Balls','Balls',(#14181));
#14141=PRODUCT_RELATED_PRODUCT_CATEGORY('Cage','Cage',(#14182));
#14142=PRODUCT_RELATED_PRODUCT_CATEGORY('Seals 2RS','Seals 2RS',(#14183));
#14143=PRODUCT_RELATED_PRODUCT_CATEGORY('Inner race spacer (1)',
'Inner race spacer (1)',(#14184));
#14144=PRODUCT_RELATED_PRODUCT_CATEGORY('M4x10 Cap Screw',
'M4x10 Cap Screw',(#14185));
#14145=PRODUCT_RELATED_PRODUCT_CATEGORY('Axle keeper (1)',
'Axle keeper (1)',(#14186));
#14146=PRODUCT_RELATED_PRODUCT_CATEGORY('Captive slot nut',
'Captive slot nut',(#14187));
#14147=PRODUCT_RELATED_PRODUCT_CATEGORY('M5x14 Cap Screw',
'M5x14 Cap Screw',(#14188));
#14148=PRODUCT_RELATED_PRODUCT_CATEGORY('Axle support (1)',
'Axle support (1)',(#14189));
#14149=APPLICATION_PROTOCOL_DEFINITION('international standard',
'automotive_design',2009,#14150);
#14150=APPLICATION_CONTEXT(
'Core Data for Automotive Mechanical Design Process');
#14151=PRODUCT_CONTEXT('part definition',#14150,'mechanical');
#14152=PRODUCT('Gravity roller conveyor section',
'PAT-047',
'Gravity roller conveyor section',(#14151));
#14153=PRODUCT('Conveyor frame','Conveyor frame','Conveyor frame',(#14151));
#14154=PRODUCT('Rail splice plate','Rail splice plate',
'Rail splice plate',(#14151));
#14155=PRODUCT('Drilled 400 mm rail','Drilled 400 mm rail',
'Drilled 400 mm rail',(#14151));
#14156=PRODUCT('Drilled 200 mm rail','Drilled 200 mm rail',
'Drilled 200 mm rail',(#14151));
#14157=PRODUCT('Slotted Extrusion - 20 x 20 x 200 mm',
'Slotted Extrusion - 20 x 20 x 200 mm',
'Slotted Extrusion - 20 x 20 x 200 mm',(#14151));
#14158=PRODUCT('M5x40 leg screw','M5x40 leg screw','M5x40 leg screw',(#14151));
#14159=PRODUCT('Cap Screw - M5x20','Cap Screw - M5x20',
'Cap Screw - M5x20',(#14151));
#14160=PRODUCT('Rail splice plate_1','Rail splice plate (1)',
'Rail splice plate',(#14151));
#14161=PRODUCT('Flat Washer - M5','Flat Washer - M5','Flat Washer - M5',
(#14151));
#14162=PRODUCT('Cross foot','Cross foot','Cross foot',(#14151));
#14163=PRODUCT('Bonded foot pad','Bonded foot pad','Bonded foot pad',(#14151));
#14164=PRODUCT('Bonded foot pad_1','Bonded foot pad (1)',
'Bonded foot pad',(#14151));
#14165=PRODUCT('Cross foot_1','Cross foot (1)','Cross foot',(#14151));
#14166=PRODUCT('Bonded foot pad_2','Bonded foot pad (2)',
'Bonded foot pad',(#14151));
#14167=PRODUCT('Bonded foot pad_3','Bonded foot pad (3)',
'Bonded foot pad',(#14151));
#14168=PRODUCT('Roller 1','Roller 1','Roller 1',(#14151));
#14169=PRODUCT('Roller tube','Roller tube','Roller tube',(#14151));
#14170=PRODUCT('Bearing insert','Bearing insert','Bearing insert',(#14151));
#14171=PRODUCT('Bearing retainer','Bearing retainer','Bearing retainer',
(#14151));
#14172=PRODUCT('Bearing insert_1','Bearing insert (1)','Bearing insert',
(#14151));
#14173=PRODUCT('Bearing retainer_1','Bearing retainer (1)',
'Bearing retainer',(#14151));
#14174=PRODUCT('Dead axle','Dead axle','Dead axle',(#14151));
#14175=PRODUCT('Axle support','Axle support','Axle support',(#14151));
#14176=PRODUCT('Axle keeper','Axle keeper','Axle keeper',(#14151));
#14177=PRODUCT('Inner race spacer','Inner race spacer',
'Inner race spacer',(#14151));
#14178=PRODUCT('Sealed Ball Bearing - 10 x 30 x 9 mm',
'Sealed Ball Bearing - 10 x 30 x 9 mm',
'Sealed Ball Bearing - 10 x 30 x 9 mm',(#14151));
#14179=PRODUCT('Inner ring','Inner ring','Inner ring',(#14151));
#14180=PRODUCT('Outer ring','Outer ring','Outer ring',(#14151));
#14181=PRODUCT('Balls','Balls','Balls',(#14151));
#14182=PRODUCT('Cage','Cage','Cage',(#14151));
#14183=PRODUCT('Seals 2RS','Seals 2RS','Seals 2RS',(#14151));
#14184=PRODUCT('Inner race spacer_1','Inner race spacer (1)',
'Inner race spacer',(#14151));
#14185=PRODUCT('M4x10 Cap Screw','M4x10 Cap Screw','M4x10 Cap Screw',(#14151));
#14186=PRODUCT('Axle keeper_1','Axle keeper (1)','Axle keeper',(#14151));
#14187=PRODUCT('Captive slot nut','Captive slot nut','Captive slot nut',
(#14151));
#14188=PRODUCT('M5x14 Cap Screw','M5x14 Cap Screw','M5x14 Cap Screw',(#14151));
#14189=PRODUCT('Axle support_1','Axle support (1)','Axle support',(#14151));
#14190=PRESENTATION_STYLE_ASSIGNMENT((#14195));
#14191=PRESENTATION_STYLE_ASSIGNMENT((#14196));
#14192=PRESENTATION_STYLE_ASSIGNMENT((#14197));
#14193=PRESENTATION_STYLE_ASSIGNMENT((#14198));
#14194=PRESENTATION_STYLE_ASSIGNMENT((#14199));
#14195=SURFACE_STYLE_USAGE(.BOTH.,#14200);
#14196=SURFACE_STYLE_USAGE(.BOTH.,#14201);
#14197=SURFACE_STYLE_USAGE(.BOTH.,#14202);
#14198=SURFACE_STYLE_USAGE(.BOTH.,#14203);
#14199=SURFACE_STYLE_USAGE(.BOTH.,#14204);
#14200=SURFACE_SIDE_STYLE('',(#14205));
#14201=SURFACE_SIDE_STYLE('',(#14206));
#14202=SURFACE_SIDE_STYLE('',(#14207));
#14203=SURFACE_SIDE_STYLE('',(#14208));
#14204=SURFACE_SIDE_STYLE('',(#14209));
#14205=SURFACE_STYLE_FILL_AREA(#14210);
#14206=SURFACE_STYLE_FILL_AREA(#14211);
#14207=SURFACE_STYLE_FILL_AREA(#14212);
#14208=SURFACE_STYLE_FILL_AREA(#14213);
#14209=SURFACE_STYLE_FILL_AREA(#14214);
#14210=FILL_AREA_STYLE('Steel - Satin',(#14215));
#14211=FILL_AREA_STYLE('CAD Library Painted - Steel gray',(#14216));
#14212=FILL_AREA_STYLE('CAD Library Painted - Engineering blue',(#14217));
#14213=FILL_AREA_STYLE('CAD Library Painted - Graphite',(#14218));
#14214=FILL_AREA_STYLE('CAD Library Painted - Deep blue',(#14219));
#14215=FILL_AREA_STYLE_COLOUR('Steel - Satin',#14220);
#14216=FILL_AREA_STYLE_COLOUR('CAD Library Painted - Steel gray',#14221);
#14217=FILL_AREA_STYLE_COLOUR('CAD Library Painted - Engineering blue',
#14222);
#14218=FILL_AREA_STYLE_COLOUR('CAD Library Painted - Graphite',#14223);
#14219=FILL_AREA_STYLE_COLOUR('CAD Library Painted - Deep blue',#14224);
#14220=COLOUR_RGB('Steel - Satin',0.627450980392157,0.627450980392157,0.627450980392157);
#14221=COLOUR_RGB('CAD Library Painted - Steel gray',0.592156862745098,
0.631372549019608,0.67843137254902);
#14222=COLOUR_RGB('CAD Library Painted - Engineering blue',0.12156862745098,
0.356862745098039,0.6);
#14223=COLOUR_RGB('CAD Library Painted - Graphite',0.168627450980392,0.192156862745098,
0.231372549019608);
#14224=COLOUR_RGB('CAD Library Painted - Deep blue',0.0784313725490196,
0.203921568627451,0.349019607843137);
ENDSEC;
END-ISO-10303-21;
